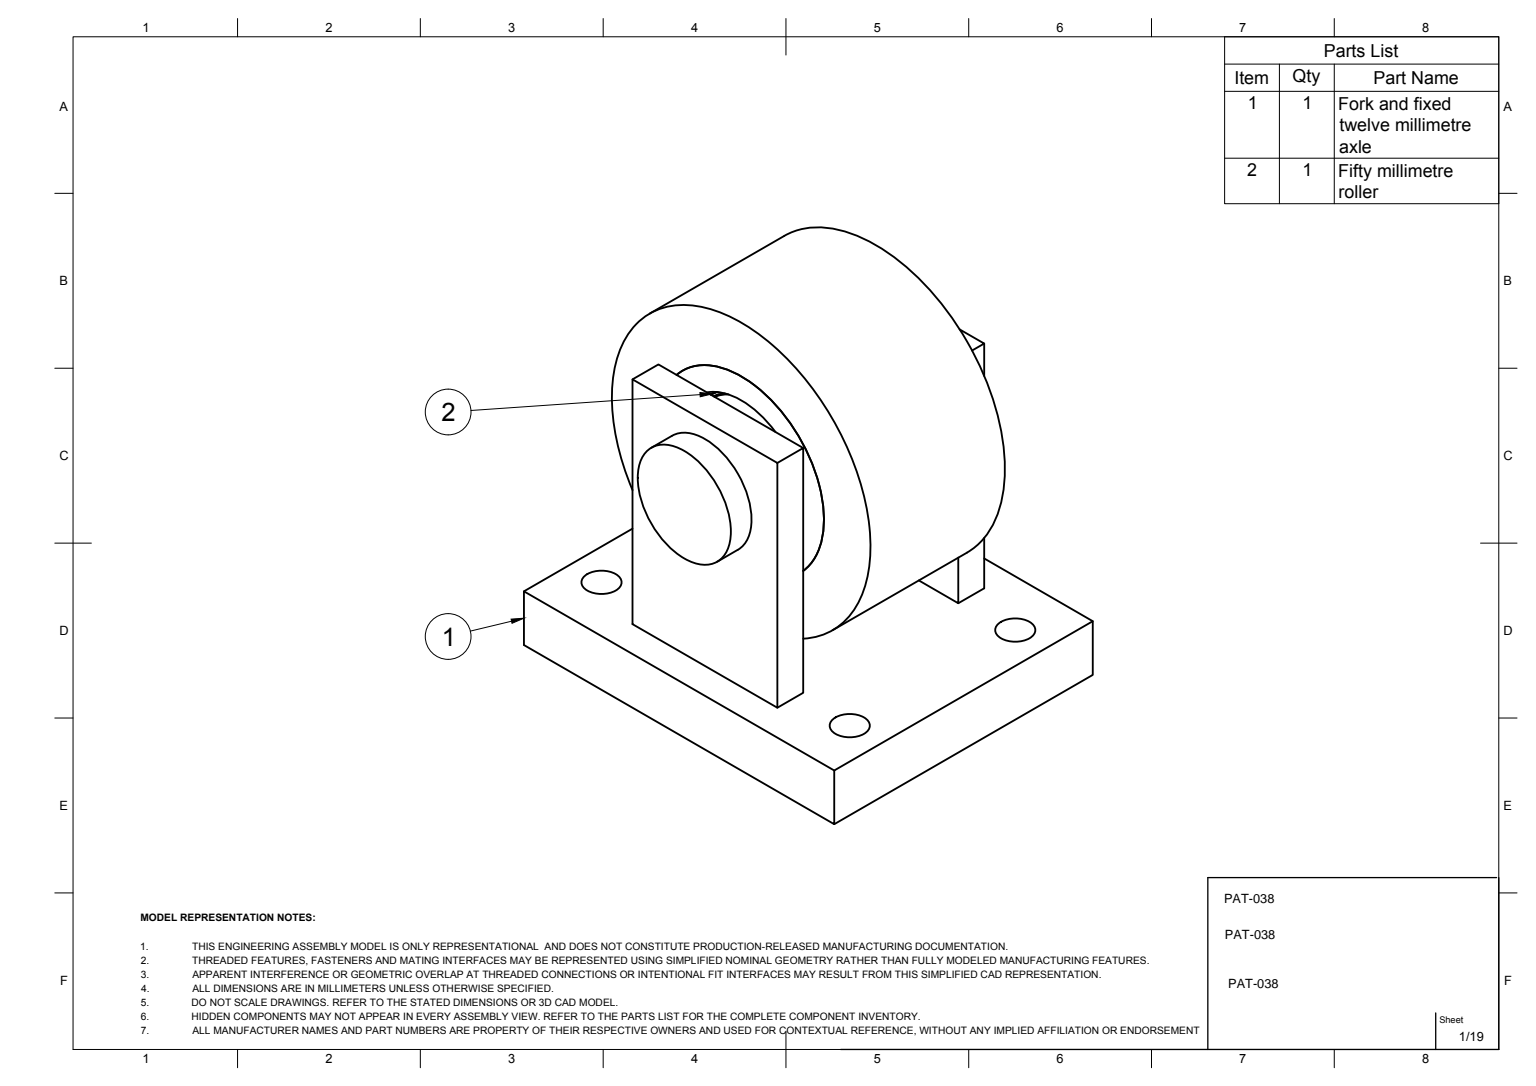
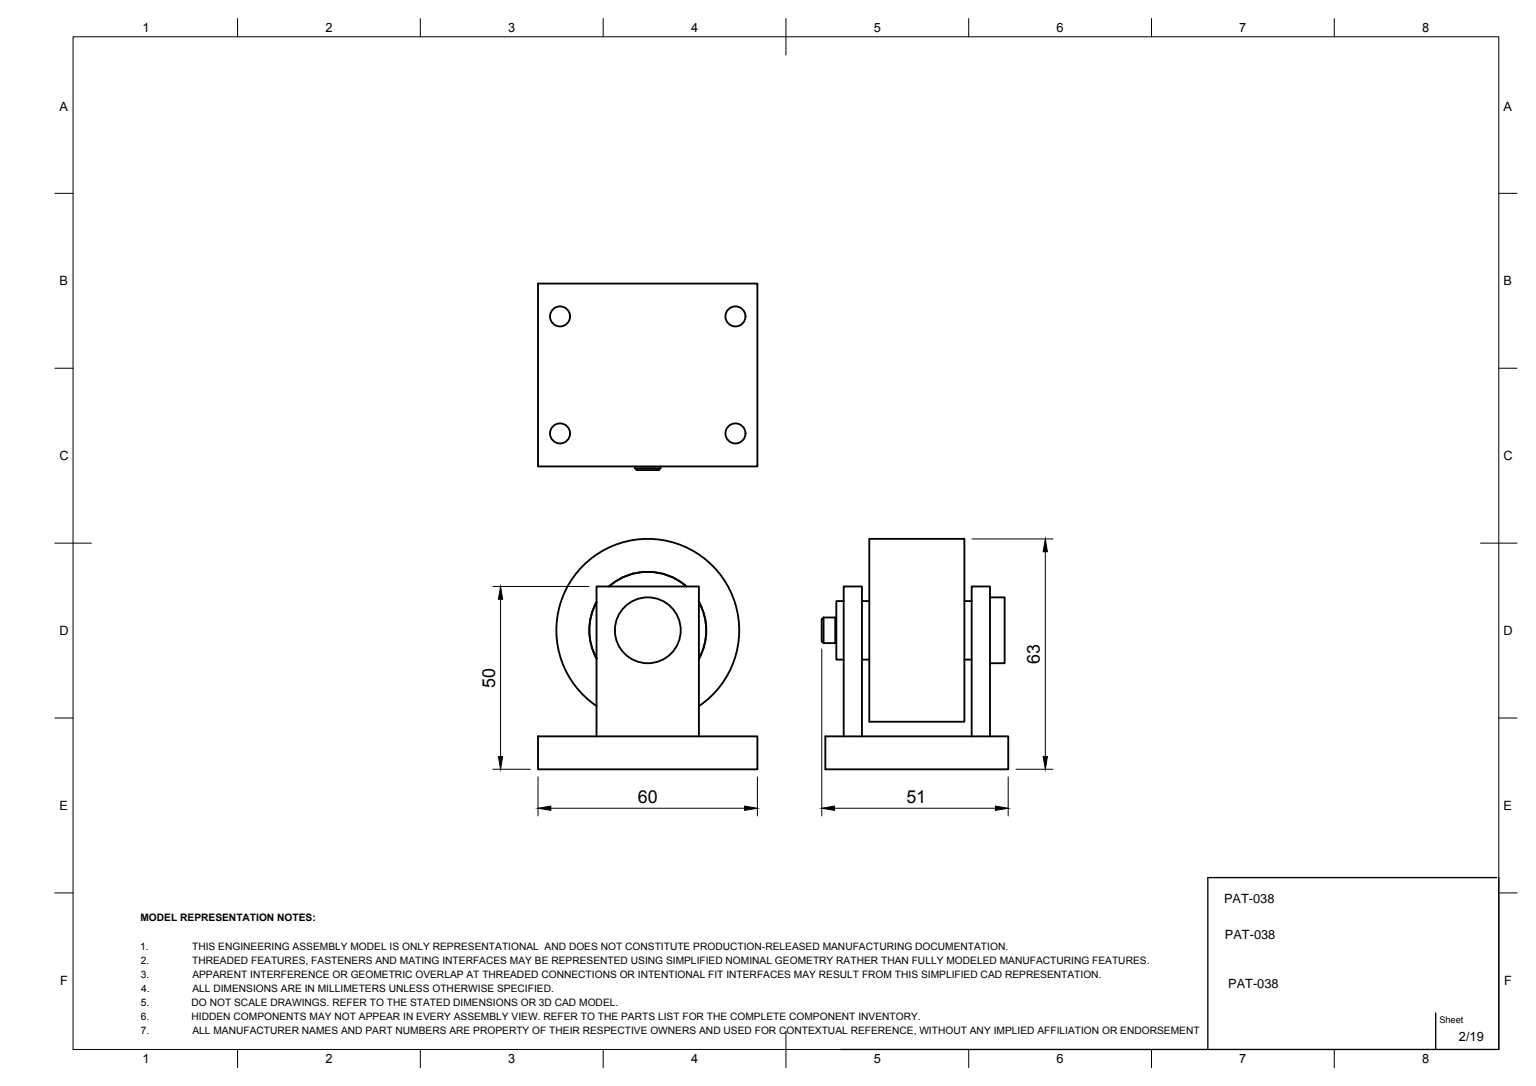
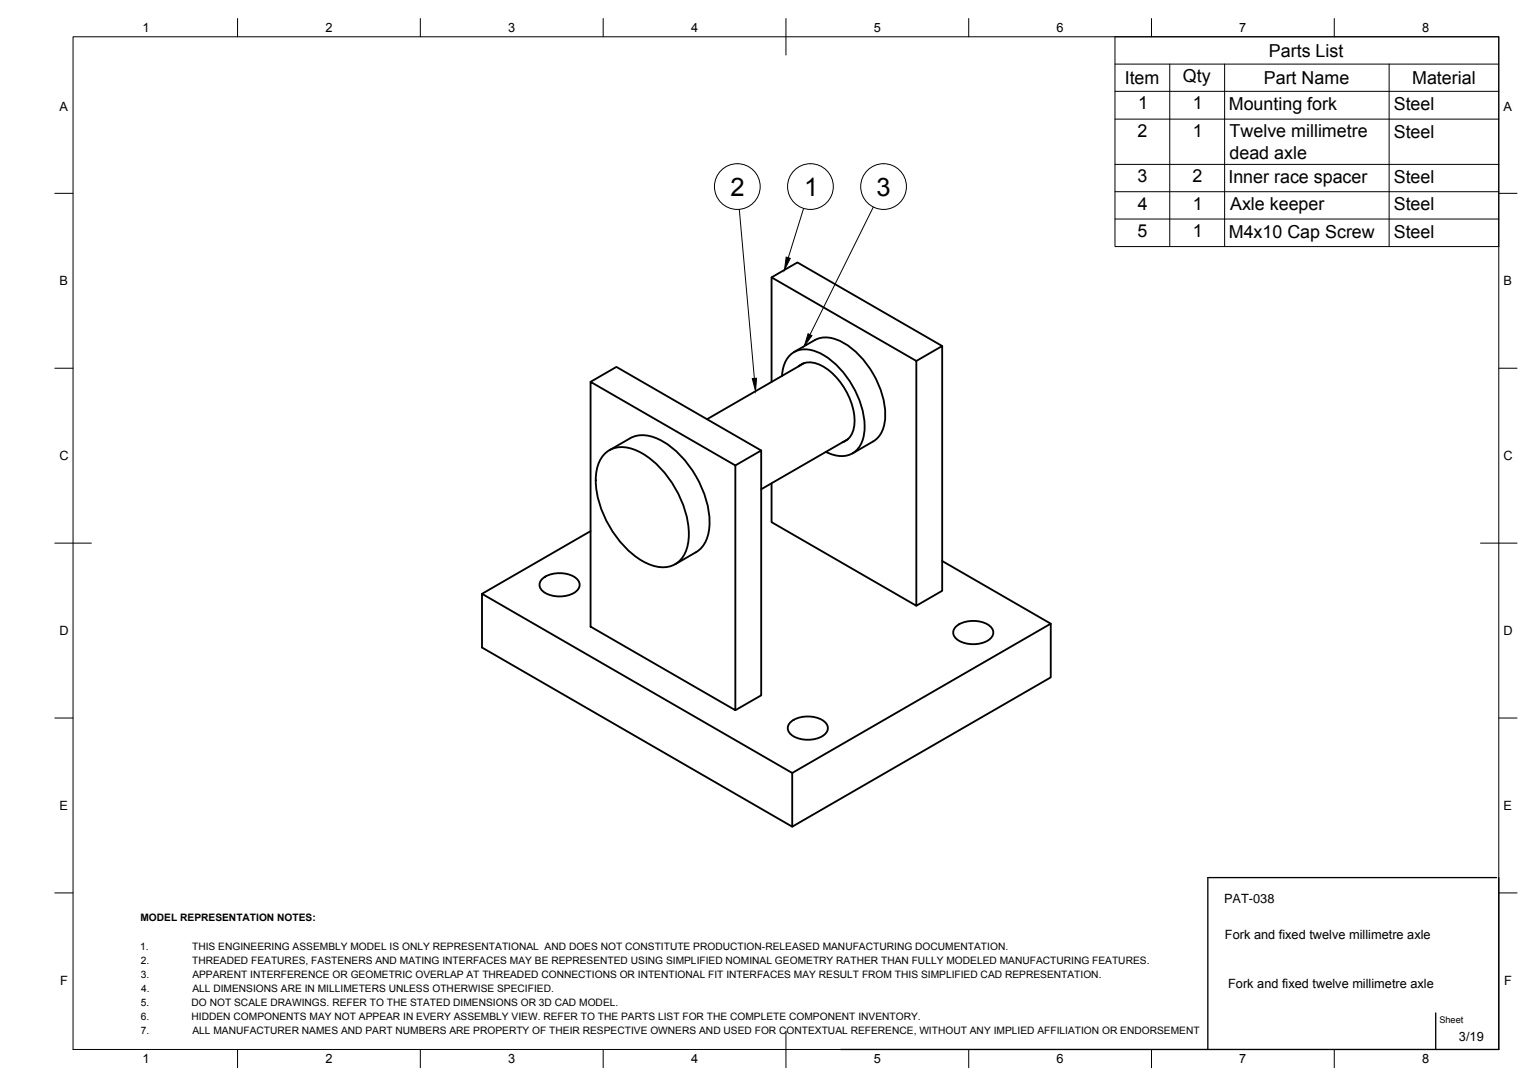
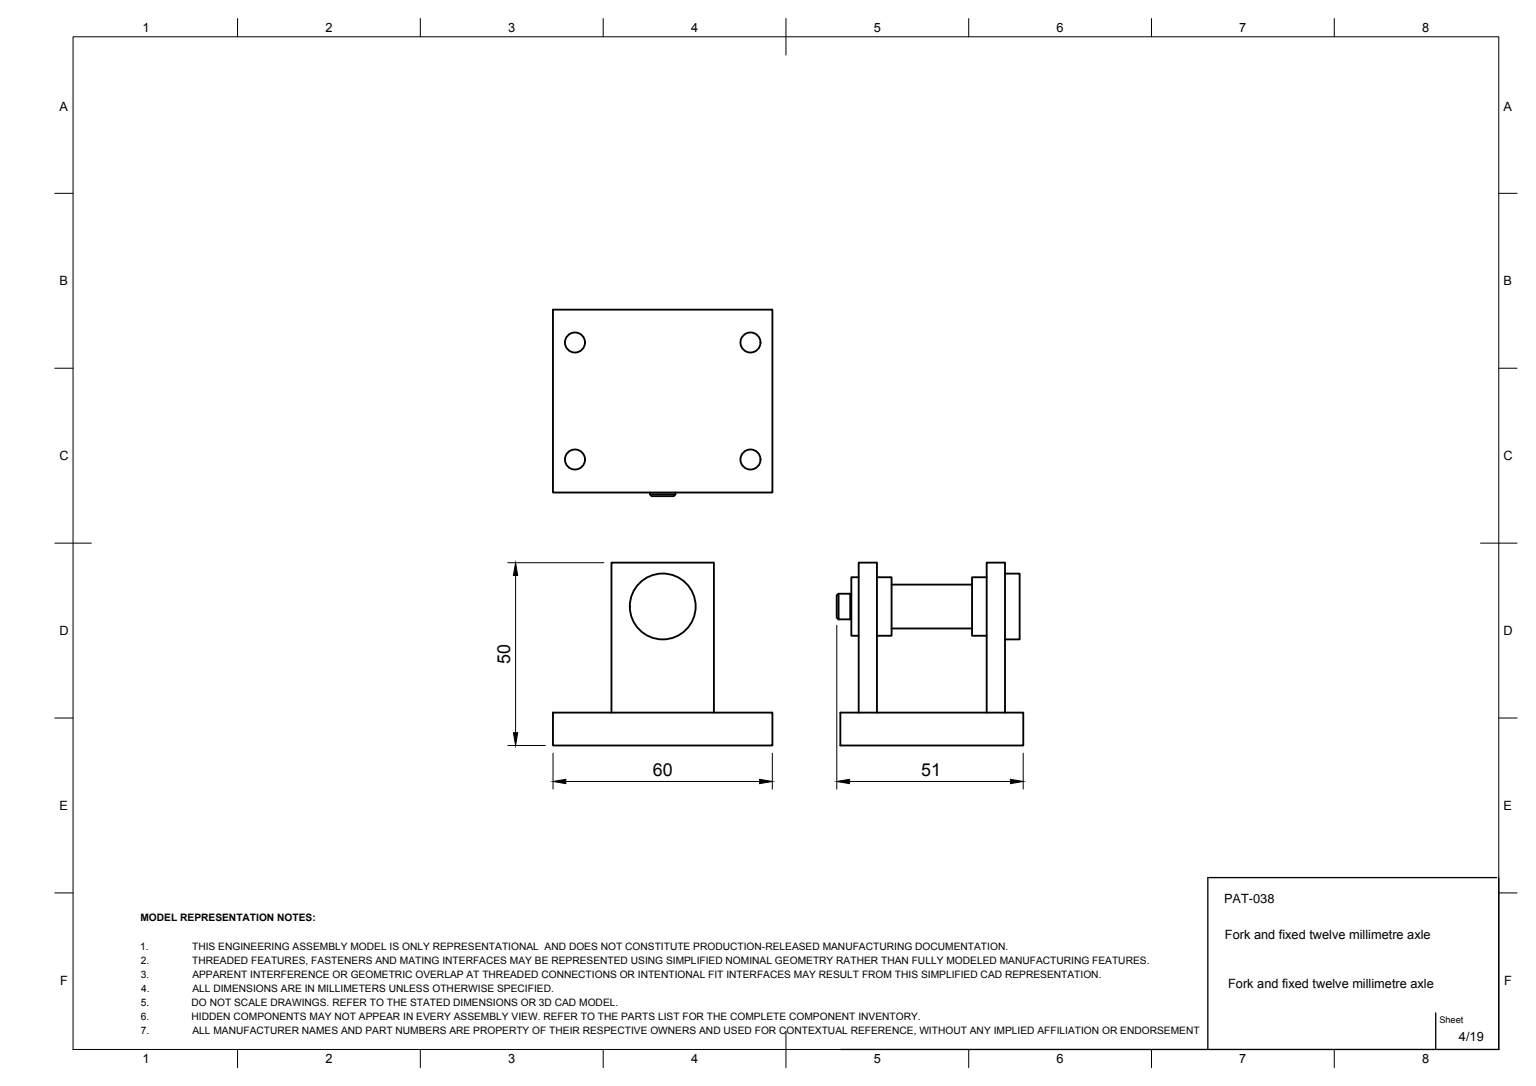
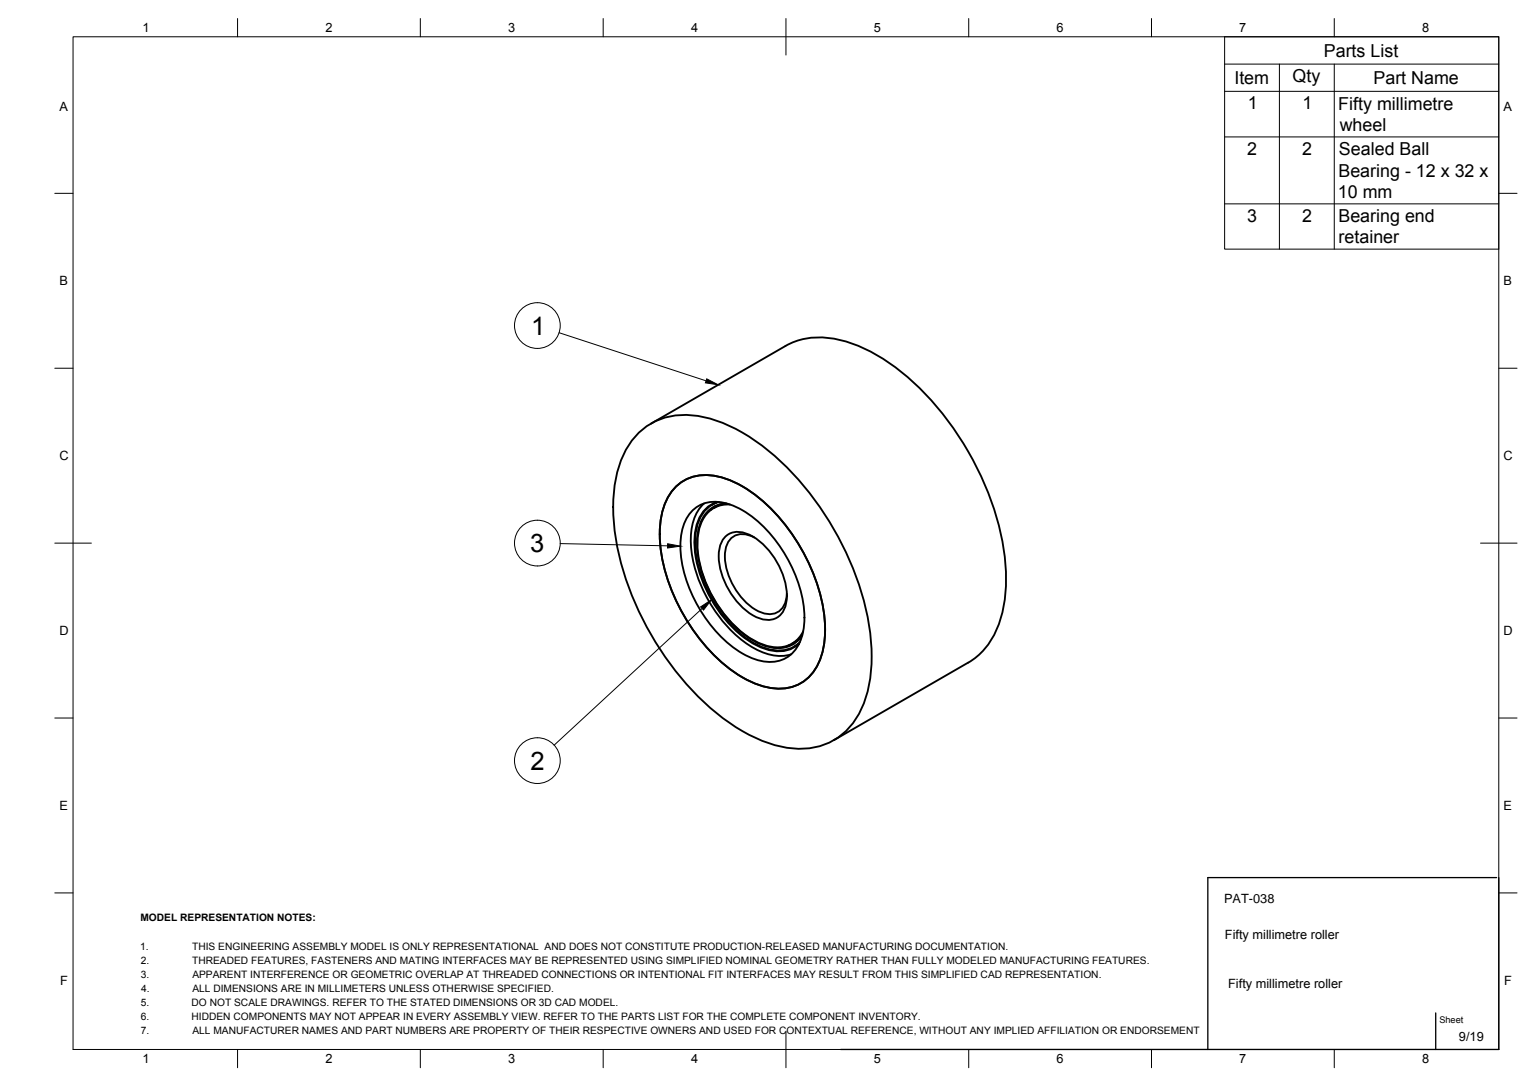
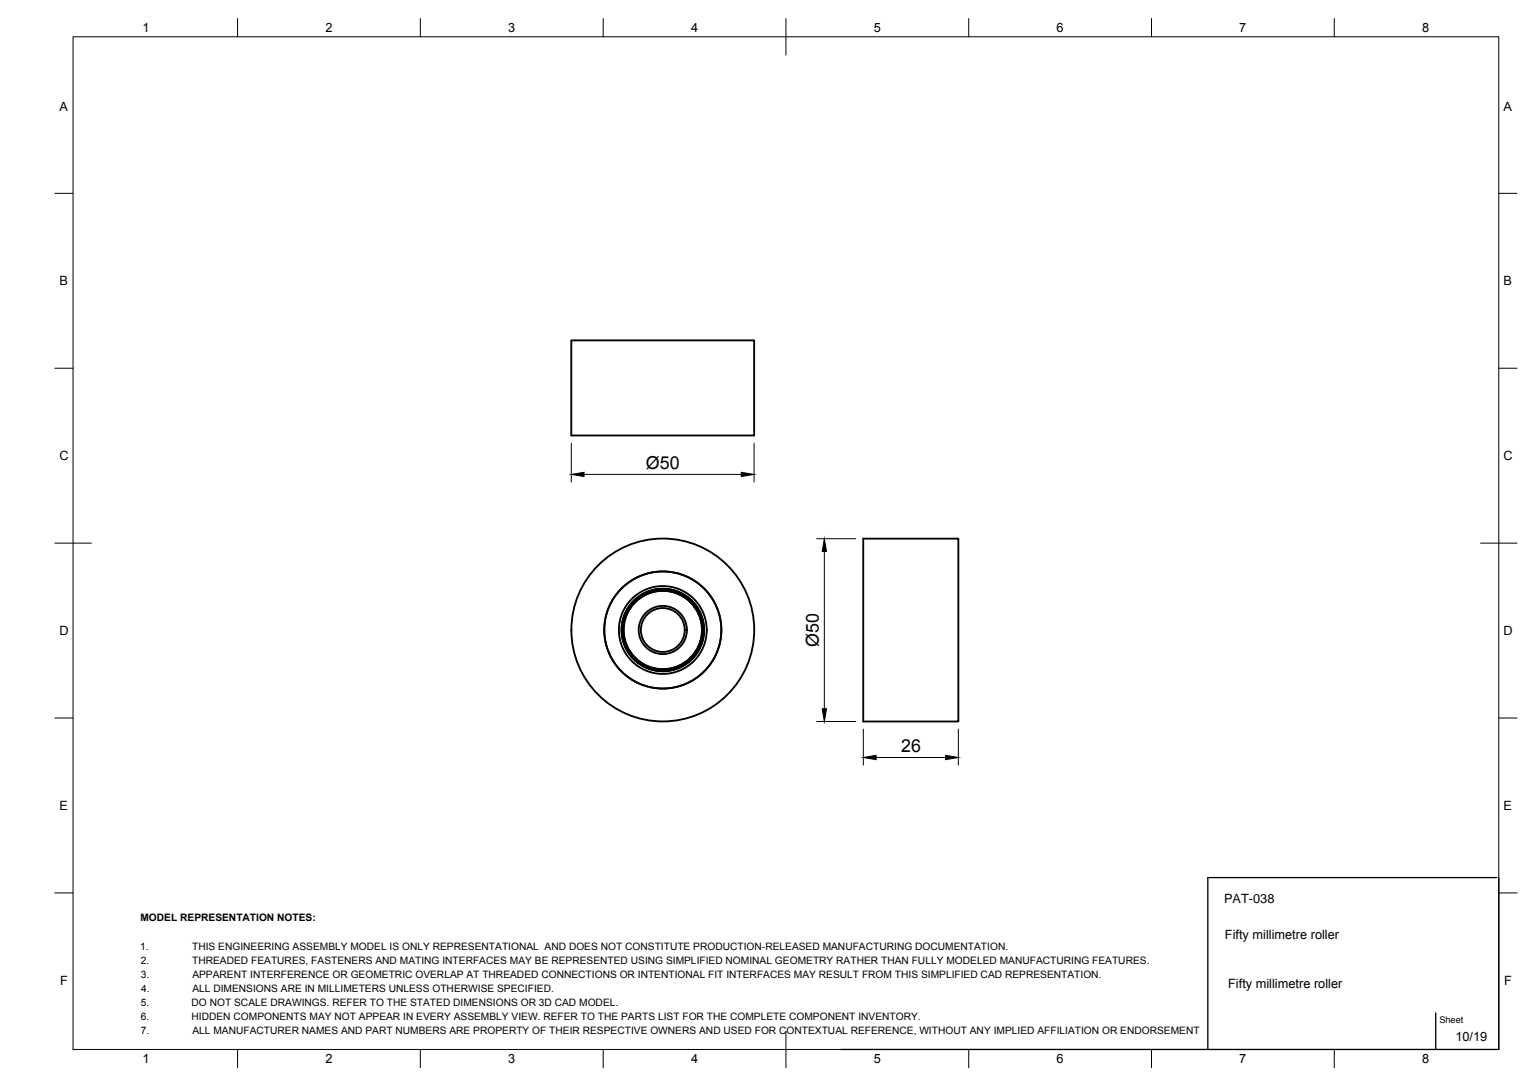
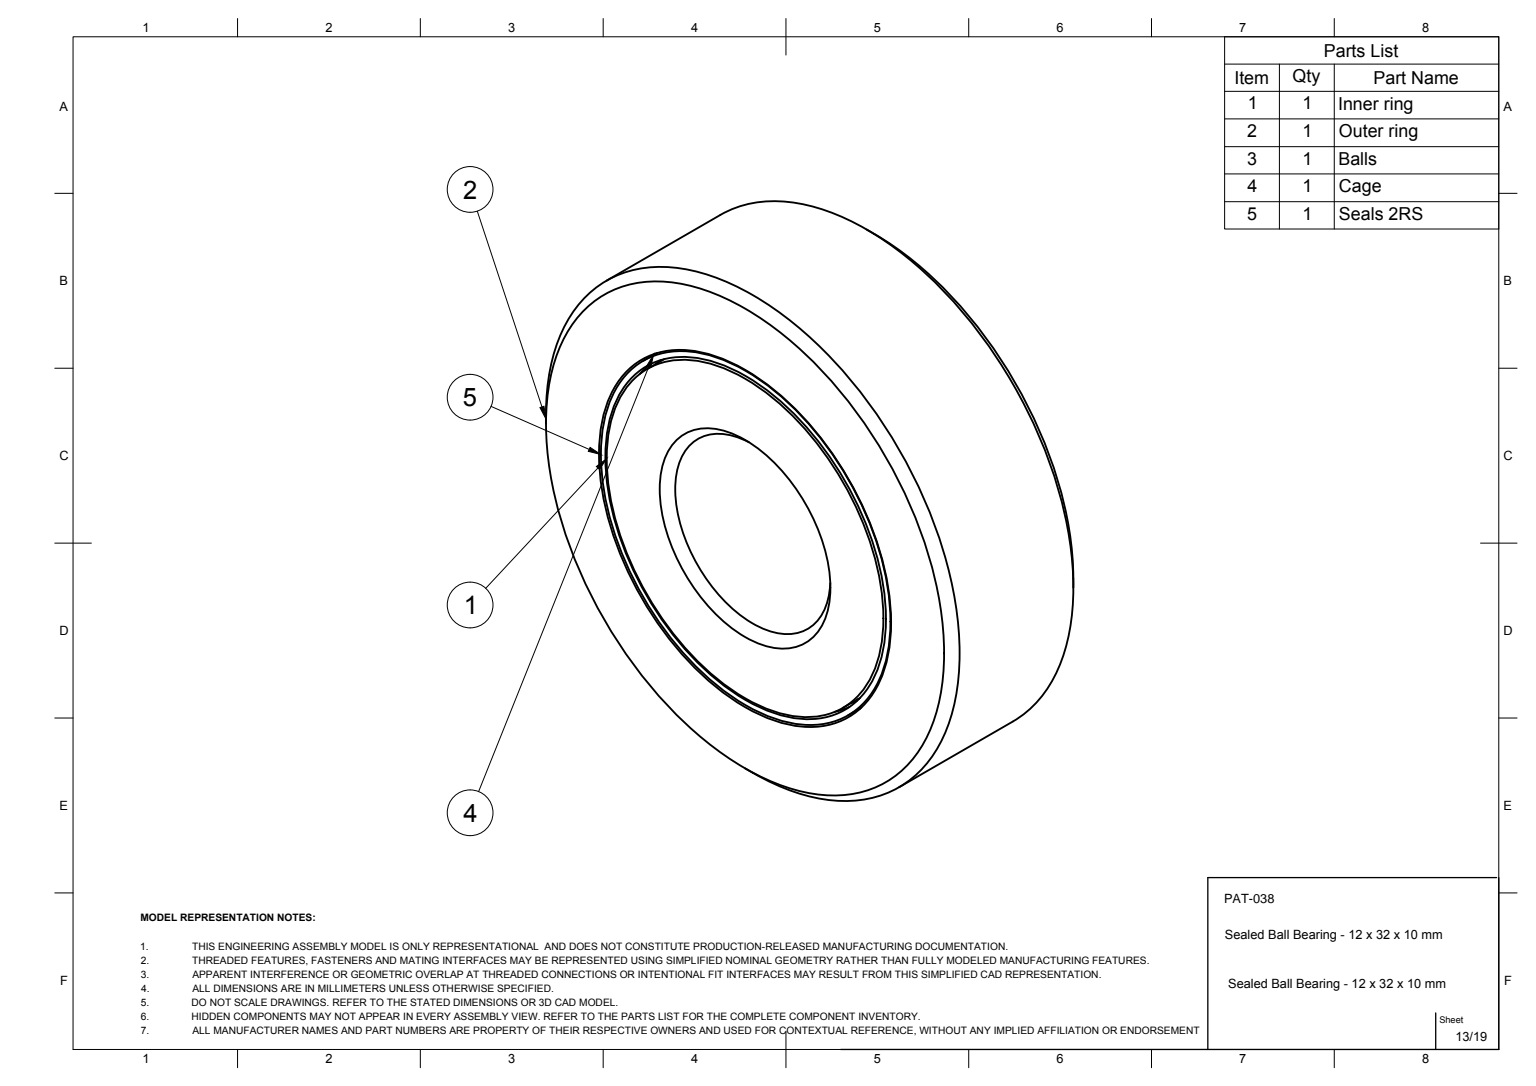
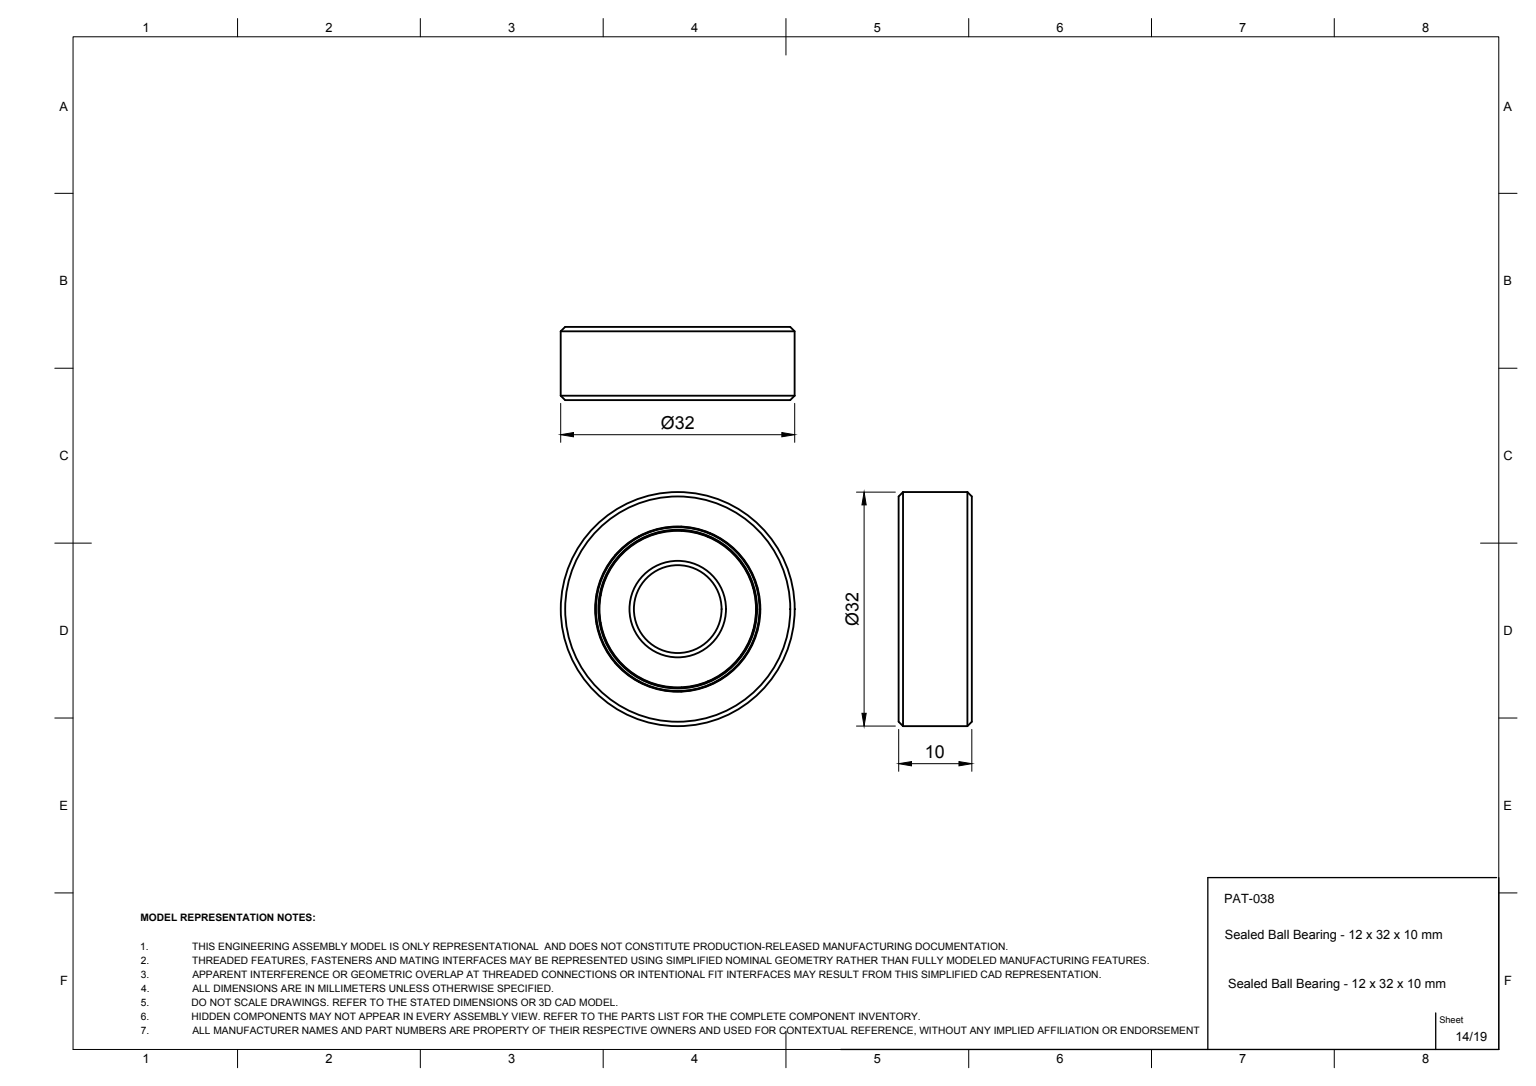
ISO-10303-21;
HEADER;
/* Generated by software containing ST-Developer
 * from STEP Tools, Inc. (www.steptools.com) 
 */

FILE_DESCRIPTION(
/* description */ ('Fork-mounted skate wheel'),
/* implementation_level */ '2;1');

FILE_NAME(
/* name */ 'PAT-038',
/* time_stamp */ '2026-10-29T16:11:26-07:00',
/* author */ (''),
/* organization */ (''),
/* preprocessor_version */ 'ST-DEVELOPER v20.2',
/* originating_system */ 'Autodesk Translation Framework v15.17.0.0',
/* authorisation */ '');

FILE_SCHEMA (('AUTOMOTIVE_DESIGN { 1 0 10303 214 3 1 1 }'));
ENDSEC;

DATA;
#10=MECHANICAL_DESIGN_GEOMETRIC_PRESENTATION_REPRESENTATION('',(#146,#147,
#148,#149,#150,#151,#152,#153,#154,#155,#156,#157,#158,#159,#160,#161,#162,
#163,#164),#3688);
#11=B_SPLINE_CURVE_WITH_KNOTS('',3,(#3211,#3212,#3213,#3214,#3215,#3216,
#3217,#3218,#3219,#3220,#3221,#3222,#3223,#3224,#3225,#3226,#3227,#3228,
#3229,#3230,#3231,#3232),.UNSPECIFIED.,.F.,.F.,(4,2,2,2,2,2,2,2,2,2,4),
(0.0591825211272536,0.157966726598481,0.236950089897721,0.315933453196962,
0.391576304923761,0.46721915665056,0.54286200837736,0.618504860104159,0.697488223403399,
0.77647158670264,0.875255792173867),.UNSPECIFIED.);
#12=B_SPLINE_CURVE_WITH_KNOTS('',3,(#3236,#3237,#3238,#3239,#3240,#3241,
#3242,#3243,#3244,#3245,#3246,#3247,#3248,#3249,#3250,#3251,#3252,#3253,
#3254,#3255,#3256,#3257),.UNSPECIFIED.,.F.,.F.,(4,2,2,2,2,2,2,2,2,2,4),
(0.0581119756758434,0.106553146291161,0.213106292582322,0.30849933801665,
0.386091982889075,0.4636846277615,0.541277272633925,0.61886991750635,0.714262962940678,
0.820816109231839,0.869257279847157),.UNSPECIFIED.);
#13=B_SPLINE_CURVE_WITH_KNOTS('',3,(#3263,#3264,#3265,#3266,#3267,#3268,
#3269,#3270,#3271,#3272,#3273,#3274,#3275,#3276,#3277,#3278,#3279,#3280,
#3281,#3282,#3283,#3284),.UNSPECIFIED.,.F.,.F.,(4,2,2,2,2,2,2,2,2,2,4),
(0.0581119756758434,0.106553146291161,0.213106292582322,0.30849933801665,
0.386091982889075,0.4636846277615,0.541277272633925,0.61886991750635,0.714262962940679,
0.820816109231839,0.869257279847157),.UNSPECIFIED.);
#14=B_SPLINE_CURVE_WITH_KNOTS('',3,(#3288,#3289,#3290,#3291,#3292,#3293,
#3294,#3295,#3296,#3297,#3298,#3299,#3300,#3301,#3302,#3303,#3304,#3305,
#3306,#3307,#3308,#3309),.UNSPECIFIED.,.F.,.F.,(4,2,2,2,2,2,2,2,2,2,4),
(0.0581119756758433,0.106553146291161,0.213106292582322,0.308499338016649,
0.386091982889075,0.4636846277615,0.541277272633925,0.61886991750635,0.714262962940678,
0.820816109231839,0.869257279847157),.UNSPECIFIED.);
#15=B_SPLINE_CURVE_WITH_KNOTS('',3,(#3318,#3319,#3320,#3321,#3322,#3323,
#3324,#3325,#3326,#3327,#3328,#3329,#3330,#3331,#3332,#3333,#3334,#3335,
#3336,#3337,#3338,#3339),.UNSPECIFIED.,.F.,.F.,(4,2,2,2,2,2,2,2,2,2,4),
(0.0581119756758433,0.106553146291161,0.213106292582322,0.30849933801665,
0.386091982889075,0.4636846277615,0.541277272633925,0.61886991750635,0.714262962940678,
0.820816109231839,0.869257279847157),.UNSPECIFIED.);
#16=B_SPLINE_CURVE_WITH_KNOTS('',3,(#3343,#3344,#3345,#3346,#3347,#3348,
#3349,#3350,#3351,#3352,#3353,#3354,#3355,#3356,#3357,#3358,#3359,#3360,
#3361,#3362,#3363,#3364),.UNSPECIFIED.,.F.,.F.,(4,2,2,2,2,2,2,2,2,2,4),
(0.0581119756758434,0.106553146291161,0.213106292582322,0.30849933801665,
0.386091982889075,0.4636846277615,0.541277272633925,0.61886991750635,0.714262962940678,
0.820816109231839,0.869257279847157),.UNSPECIFIED.);
#17=B_SPLINE_CURVE_WITH_KNOTS('',3,(#3368,#3369,#3370,#3371,#3372,#3373,
#3374,#3375,#3376,#3377,#3378,#3379,#3380,#3381,#3382,#3383,#3384,#3385,
#3386,#3387,#3388,#3389),.UNSPECIFIED.,.F.,.F.,(4,2,2,2,2,2,2,2,2,2,4),
(0.0581119756758434,0.106553146291161,0.213106292582322,0.30849933801665,
0.386091982889075,0.4636846277615,0.541277272633925,0.61886991750635,0.714262962940678,
0.820816109231839,0.869257279847157),.UNSPECIFIED.);
#18=B_SPLINE_CURVE_WITH_KNOTS('',3,(#3393,#3394,#3395,#3396,#3397,#3398,
#3399,#3400,#3401,#3402,#3403,#3404,#3405,#3406,#3407,#3408,#3409,#3410,
#3411,#3412,#3413,#3414),.UNSPECIFIED.,.F.,.F.,(4,2,2,2,2,2,2,2,2,2,4),
(0.0581119756758433,0.106553146291161,0.213106292582322,0.30849933801665,
0.386091982889075,0.4636846277615,0.541277272633925,0.61886991750635,0.714262962940678,
0.820816109231839,0.869257279847157),.UNSPECIFIED.);
#19=B_SPLINE_CURVE_WITH_KNOTS('',3,(#3422,#3423,#3424,#3425,#3426,#3427,
#3428,#3429,#3430,#3431,#3432,#3433,#3434,#3435,#3436,#3437,#3438,#3439,
#3440,#3441,#3442,#3443),.UNSPECIFIED.,.F.,.F.,(4,2,2,2,2,2,2,2,2,2,4),
(0.0591825211272536,0.157966726598481,0.236950089897721,0.315933453196962,
0.391576304923761,0.467219156650561,0.54286200837736,0.618504860104159,
0.697488223403399,0.77647158670264,0.875255792173867),.UNSPECIFIED.);
#20=B_SPLINE_CURVE_WITH_KNOTS('',3,(#3451,#3452,#3453,#3454,#3455,#3456,
#3457,#3458,#3459,#3460,#3461,#3462,#3463,#3464,#3465,#3466,#3467,#3468,
#3469,#3470,#3471,#3472),.UNSPECIFIED.,.F.,.F.,(4,2,2,2,2,2,2,2,2,2,4),
(0.0591825211272536,0.157966726598481,0.236950089897722,0.315933453196962,
0.391576304923761,0.467219156650561,0.54286200837736,0.618504860104159,
0.697488223403399,0.77647158670264,0.875255792173867),.UNSPECIFIED.);
#21=B_SPLINE_CURVE_WITH_KNOTS('',3,(#3482,#3483,#3484,#3485,#3486,#3487,
#3488,#3489,#3490,#3491,#3492,#3493,#3494,#3495,#3496,#3497,#3498,#3499,
#3500,#3501,#3502,#3503),.UNSPECIFIED.,.F.,.F.,(4,2,2,2,2,2,2,2,2,2,4),
(0.0591825211272536,0.157966726598481,0.236950089897721,0.315933453196962,
0.391576304923761,0.46721915665056,0.54286200837736,0.618504860104159,0.697488223403399,
0.77647158670264,0.875255792173867),.UNSPECIFIED.);
#22=B_SPLINE_CURVE_WITH_KNOTS('',3,(#3511,#3512,#3513,#3514,#3515,#3516,
#3517,#3518,#3519,#3520,#3521,#3522,#3523,#3524,#3525,#3526,#3527,#3528,
#3529,#3530,#3531,#3532),.UNSPECIFIED.,.F.,.F.,(4,2,2,2,2,2,2,2,2,2,4),
(0.0591825211272536,0.157966726598481,0.236950089897721,0.315933453196962,
0.391576304923761,0.46721915665056,0.542862008377359,0.618504860104159,
0.697488223403399,0.776471586702639,0.875255792173867),.UNSPECIFIED.);
#23=B_SPLINE_CURVE_WITH_KNOTS('',3,(#3540,#3541,#3542,#3543,#3544,#3545,
#3546,#3547,#3548,#3549,#3550,#3551,#3552,#3553,#3554,#3555,#3556,#3557,
#3558,#3559,#3560,#3561),.UNSPECIFIED.,.F.,.F.,(4,2,2,2,2,2,2,2,2,2,4),
(0.0591825211272536,0.157966726598481,0.236950089897721,0.315933453196962,
0.391576304923761,0.46721915665056,0.54286200837736,0.618504860104159,0.697488223403399,
0.77647158670264,0.875255792173867),.UNSPECIFIED.);
#24=B_SPLINE_CURVE_WITH_KNOTS('',3,(#3570,#3571,#3572,#3573,#3574,#3575,
#3576,#3577,#3578,#3579,#3580,#3581,#3582,#3583,#3584,#3585,#3586,#3587,
#3588,#3589,#3590,#3591),.UNSPECIFIED.,.F.,.F.,(4,2,2,2,2,2,2,2,2,2,4),
(0.0591825211272536,0.157966726598481,0.236950089897721,0.315933453196962,
0.391576304923761,0.46721915665056,0.542862008377359,0.618504860104159,
0.697488223403399,0.776471586702639,0.875255792173867),.UNSPECIFIED.);
#25=SPHERICAL_SURFACE('',#2119,0.29765);
#26=SPHERICAL_SURFACE('',#2121,0.29765);
#27=SPHERICAL_SURFACE('',#2123,0.29765);
#28=SPHERICAL_SURFACE('',#2125,0.29765);
#29=SPHERICAL_SURFACE('',#2127,0.29765);
#30=SPHERICAL_SURFACE('',#2129,0.29765);
#31=SPHERICAL_SURFACE('',#2131,0.29765);
#32=SPHERICAL_SURFACE('',#2134,0.309556);
#33=SPHERICAL_SURFACE('',#2150,0.309556);
#34=SPHERICAL_SURFACE('',#2155,0.309556);
#35=SPHERICAL_SURFACE('',#2161,0.309556);
#36=SPHERICAL_SURFACE('',#2166,0.309556);
#37=SPHERICAL_SURFACE('',#2171,0.309556);
#38=SPHERICAL_SURFACE('',#2179,0.309556);
#39=TOROIDAL_SURFACE('',#2079,1.1,0.309556);
#40=TOROIDAL_SURFACE('',#2099,1.1,0.309556);
#41=ITEM_DEFINED_TRANSFORMATION($,$,#1962,#2053);
#42=ITEM_DEFINED_TRANSFORMATION($,$,#1997,#2054);
#43=ITEM_DEFINED_TRANSFORMATION($,$,#2011,#2055);
#44=ITEM_DEFINED_TRANSFORMATION($,$,#2011,#2056);
#45=ITEM_DEFINED_TRANSFORMATION($,$,#2020,#2057);
#46=ITEM_DEFINED_TRANSFORMATION($,$,#2029,#2058);
#47=ITEM_DEFINED_TRANSFORMATION($,$,#2078,#2200);
#48=ITEM_DEFINED_TRANSFORMATION($,$,#2098,#2201);
#49=ITEM_DEFINED_TRANSFORMATION($,$,#2118,#2202);
#50=ITEM_DEFINED_TRANSFORMATION($,$,#2133,#2203);
#51=ITEM_DEFINED_TRANSFORMATION($,$,#2183,#2204);
#52=ITEM_DEFINED_TRANSFORMATION($,$,#2060,#2214);
#53=ITEM_DEFINED_TRANSFORMATION($,$,#2205,#2215);
#54=ITEM_DEFINED_TRANSFORMATION($,$,#2077,#2216);
#55=ITEM_DEFINED_TRANSFORMATION($,$,#2077,#2217);
#56=ITEM_DEFINED_TRANSFORMATION($,$,#2205,#2218);
#57=ITEM_DEFINED_TRANSFORMATION($,$,#1961,#2219);
#58=ITEM_DEFINED_TRANSFORMATION($,$,#2059,#2220);
#59=(
REPRESENTATION_RELATIONSHIP($,$,#3745,#3744)
REPRESENTATION_RELATIONSHIP_WITH_TRANSFORMATION(#41)
SHAPE_REPRESENTATION_RELATIONSHIP()
);
#60=(
REPRESENTATION_RELATIONSHIP($,$,#3746,#3744)
REPRESENTATION_RELATIONSHIP_WITH_TRANSFORMATION(#42)
SHAPE_REPRESENTATION_RELATIONSHIP()
);
#61=(
REPRESENTATION_RELATIONSHIP($,$,#3747,#3744)
REPRESENTATION_RELATIONSHIP_WITH_TRANSFORMATION(#43)
SHAPE_REPRESENTATION_RELATIONSHIP()
);
#62=(
REPRESENTATION_RELATIONSHIP($,$,#3747,#3744)
REPRESENTATION_RELATIONSHIP_WITH_TRANSFORMATION(#44)
SHAPE_REPRESENTATION_RELATIONSHIP()
);
#63=(
REPRESENTATION_RELATIONSHIP($,$,#3748,#3744)
REPRESENTATION_RELATIONSHIP_WITH_TRANSFORMATION(#45)
SHAPE_REPRESENTATION_RELATIONSHIP()
);
#64=(
REPRESENTATION_RELATIONSHIP($,$,#3749,#3744)
REPRESENTATION_RELATIONSHIP_WITH_TRANSFORMATION(#46)
SHAPE_REPRESENTATION_RELATIONSHIP()
);
#65=(
REPRESENTATION_RELATIONSHIP($,$,#3753,#3752)
REPRESENTATION_RELATIONSHIP_WITH_TRANSFORMATION(#47)
SHAPE_REPRESENTATION_RELATIONSHIP()
);
#66=(
REPRESENTATION_RELATIONSHIP($,$,#3754,#3752)
REPRESENTATION_RELATIONSHIP_WITH_TRANSFORMATION(#48)
SHAPE_REPRESENTATION_RELATIONSHIP()
);
#67=(
REPRESENTATION_RELATIONSHIP($,$,#3755,#3752)
REPRESENTATION_RELATIONSHIP_WITH_TRANSFORMATION(#49)
SHAPE_REPRESENTATION_RELATIONSHIP()
);
#68=(
REPRESENTATION_RELATIONSHIP($,$,#3756,#3752)
REPRESENTATION_RELATIONSHIP_WITH_TRANSFORMATION(#50)
SHAPE_REPRESENTATION_RELATIONSHIP()
);
#69=(
REPRESENTATION_RELATIONSHIP($,$,#3757,#3752)
REPRESENTATION_RELATIONSHIP_WITH_TRANSFORMATION(#51)
SHAPE_REPRESENTATION_RELATIONSHIP()
);
#70=(
REPRESENTATION_RELATIONSHIP($,$,#3751,#3750)
REPRESENTATION_RELATIONSHIP_WITH_TRANSFORMATION(#52)
SHAPE_REPRESENTATION_RELATIONSHIP()
);
#71=(
REPRESENTATION_RELATIONSHIP($,$,#3758,#3750)
REPRESENTATION_RELATIONSHIP_WITH_TRANSFORMATION(#53)
SHAPE_REPRESENTATION_RELATIONSHIP()
);
#72=(
REPRESENTATION_RELATIONSHIP($,$,#3752,#3750)
REPRESENTATION_RELATIONSHIP_WITH_TRANSFORMATION(#54)
SHAPE_REPRESENTATION_RELATIONSHIP()
);
#73=(
REPRESENTATION_RELATIONSHIP($,$,#3752,#3750)
REPRESENTATION_RELATIONSHIP_WITH_TRANSFORMATION(#55)
SHAPE_REPRESENTATION_RELATIONSHIP()
);
#74=(
REPRESENTATION_RELATIONSHIP($,$,#3758,#3750)
REPRESENTATION_RELATIONSHIP_WITH_TRANSFORMATION(#56)
SHAPE_REPRESENTATION_RELATIONSHIP()
);
#75=(
REPRESENTATION_RELATIONSHIP($,$,#3744,#3743)
REPRESENTATION_RELATIONSHIP_WITH_TRANSFORMATION(#57)
SHAPE_REPRESENTATION_RELATIONSHIP()
);
#76=(
REPRESENTATION_RELATIONSHIP($,$,#3750,#3743)
REPRESENTATION_RELATIONSHIP_WITH_TRANSFORMATION(#58)
SHAPE_REPRESENTATION_RELATIONSHIP()
);
#77=CONTEXT_DEPENDENT_SHAPE_REPRESENTATION(#59,#3716);
#78=CONTEXT_DEPENDENT_SHAPE_REPRESENTATION(#60,#3717);
#79=CONTEXT_DEPENDENT_SHAPE_REPRESENTATION(#61,#3718);
#80=CONTEXT_DEPENDENT_SHAPE_REPRESENTATION(#62,#3719);
#81=CONTEXT_DEPENDENT_SHAPE_REPRESENTATION(#63,#3720);
#82=CONTEXT_DEPENDENT_SHAPE_REPRESENTATION(#64,#3721);
#83=CONTEXT_DEPENDENT_SHAPE_REPRESENTATION(#65,#3730);
#84=CONTEXT_DEPENDENT_SHAPE_REPRESENTATION(#66,#3731);
#85=CONTEXT_DEPENDENT_SHAPE_REPRESENTATION(#67,#3732);
#86=CONTEXT_DEPENDENT_SHAPE_REPRESENTATION(#68,#3733);
#87=CONTEXT_DEPENDENT_SHAPE_REPRESENTATION(#69,#3734);
#88=CONTEXT_DEPENDENT_SHAPE_REPRESENTATION(#70,#3736);
#89=CONTEXT_DEPENDENT_SHAPE_REPRESENTATION(#71,#3737);
#90=CONTEXT_DEPENDENT_SHAPE_REPRESENTATION(#72,#3738);
#91=CONTEXT_DEPENDENT_SHAPE_REPRESENTATION(#73,#3739);
#92=CONTEXT_DEPENDENT_SHAPE_REPRESENTATION(#74,#3740);
#93=CONTEXT_DEPENDENT_SHAPE_REPRESENTATION(#75,#3741);
#94=CONTEXT_DEPENDENT_SHAPE_REPRESENTATION(#76,#3742);
#95=NEXT_ASSEMBLY_USAGE_OCCURRENCE('Mounting fork:1','Mounting fork:1',
'Mounting fork:1',#3761,#3762,'Mounting fork:1');
#96=NEXT_ASSEMBLY_USAGE_OCCURRENCE('Twelve millimetre dead axle:1',
'Twelve millimetre dead axle:1','Twelve millimetre dead axle:1',#3761,#3763,
'Twelve millimetre dead axle:1');
#97=NEXT_ASSEMBLY_USAGE_OCCURRENCE('Inner race spacer:2',
'Inner race spacer:2','Inner race spacer:2',#3761,#3764,
'Inner race spacer:2');
#98=NEXT_ASSEMBLY_USAGE_OCCURRENCE('Inner race spacer:3',
'Inner race spacer:3','Inner race spacer:3',#3761,#3764,
'Inner race spacer:3');
#99=NEXT_ASSEMBLY_USAGE_OCCURRENCE('Axle keeper:2','Axle keeper:2',
'Axle keeper:2',#3761,#3765,'Axle keeper:2');
#100=NEXT_ASSEMBLY_USAGE_OCCURRENCE('M4x10 Cap Screw:2',
'M4x10 Cap Screw:2','M4x10 Cap Screw:2',#3761,#3766,'M4x10 Cap Screw:2');
#101=NEXT_ASSEMBLY_USAGE_OCCURRENCE('Inner ring:1','Inner ring:1',
'Inner ring:1',#3769,#3770,'Inner ring:1');
#102=NEXT_ASSEMBLY_USAGE_OCCURRENCE('Outer ring:1','Outer ring:1',
'Outer ring:1',#3769,#3771,'Outer ring:1');
#103=NEXT_ASSEMBLY_USAGE_OCCURRENCE('Balls:1','Balls:1','Balls:1',#3769,
#3772,'Balls:1');
#104=NEXT_ASSEMBLY_USAGE_OCCURRENCE('Cage:1','Cage:1','Cage:1',#3769,#3773,
'Cage:1');
#105=NEXT_ASSEMBLY_USAGE_OCCURRENCE('Seals 2RS:1','Seals 2RS:1',
'Seals 2RS:1',#3769,#3774,'Seals 2RS:1');
#106=NEXT_ASSEMBLY_USAGE_OCCURRENCE('Fifty millimetre wheel:1',
'Fifty millimetre wheel:1','Fifty millimetre wheel:1',#3767,#3768,
'Fifty millimetre wheel:1');
#107=NEXT_ASSEMBLY_USAGE_OCCURRENCE('Bearing end retainer:1',
'Bearing end retainer:1','Bearing end retainer:1',#3767,#3775,
'Bearing end retainer:1');
#108=NEXT_ASSEMBLY_USAGE_OCCURRENCE(
'Sealed Ball Bearing - 12 x 32 x 10 mm:2',
'Sealed Ball Bearing - 12 x 32 x 10 mm:2',
'Sealed Ball Bearing - 12 x 32 x 10 mm:2',#3767,#3769,
'Sealed Ball Bearing - 12 x 32 x 10 mm:2');
#109=NEXT_ASSEMBLY_USAGE_OCCURRENCE(
'Sealed Ball Bearing - 12 x 32 x 10 mm:3',
'Sealed Ball Bearing - 12 x 32 x 10 mm:3',
'Sealed Ball Bearing - 12 x 32 x 10 mm:3',#3767,#3769,
'Sealed Ball Bearing - 12 x 32 x 10 mm:3');
#110=NEXT_ASSEMBLY_USAGE_OCCURRENCE('Bearing end retainer:2',
'Bearing end retainer:2','Bearing end retainer:2',#3767,#3775,
'Bearing end retainer:2');
#111=NEXT_ASSEMBLY_USAGE_OCCURRENCE(
'Fork and fixed twelve millimetre axle:1',
'Fork and fixed twelve millimetre axle:1',
'Fork and fixed twelve millimetre axle:1',#3760,#3761,
'Fork and fixed twelve millimetre axle:1');
#112=NEXT_ASSEMBLY_USAGE_OCCURRENCE('Fifty millimetre roller:1',
'Fifty millimetre roller:1','Fifty millimetre roller:1',#3760,#3767,
'Fifty millimetre roller:1');
#113=CONICAL_SURFACE('',#2042,0.325,0.785398163397448);
#114=CONICAL_SURFACE('',#2046,0.335,0.785398163397448);
#115=CONICAL_SURFACE('',#2050,0.21,0.463647609000806);
#116=CONICAL_SURFACE('',#2090,0.63,0.785398163397448);
#117=CONICAL_SURFACE('',#2097,0.63,0.785398163397448);
#118=CONICAL_SURFACE('',#2110,1.57,0.785398163397449);
#119=CONICAL_SURFACE('',#2114,1.57,0.785398163397449);
#120=ORIENTED_CLOSED_SHELL('',*,#1811,.F.);
#121=BREP_WITH_VOIDS('Body1',#1812,(#120));
#122=SHAPE_REPRESENTATION_RELATIONSHIP('SRR','None',#3745,#134);
#123=SHAPE_REPRESENTATION_RELATIONSHIP('SRR','None',#3746,#135);
#124=SHAPE_REPRESENTATION_RELATIONSHIP('SRR','None',#3747,#136);
#125=SHAPE_REPRESENTATION_RELATIONSHIP('SRR','None',#3748,#137);
#126=SHAPE_REPRESENTATION_RELATIONSHIP('SRR','None',#3749,#138);
#127=SHAPE_REPRESENTATION_RELATIONSHIP('SRR','None',#3751,#139);
#128=SHAPE_REPRESENTATION_RELATIONSHIP('SRR','None',#3753,#140);
#129=SHAPE_REPRESENTATION_RELATIONSHIP('SRR','None',#3754,#141);
#130=SHAPE_REPRESENTATION_RELATIONSHIP('SRR','None',#3755,#142);
#131=SHAPE_REPRESENTATION_RELATIONSHIP('SRR','None',#3756,#143);
#132=SHAPE_REPRESENTATION_RELATIONSHIP('SRR','None',#3757,#144);
#133=SHAPE_REPRESENTATION_RELATIONSHIP('SRR','None',#3758,#145);
#134=ADVANCED_BREP_SHAPE_REPRESENTATION('',(#165),#3674);
#135=ADVANCED_BREP_SHAPE_REPRESENTATION('',(#166),#3675);
#136=ADVANCED_BREP_SHAPE_REPRESENTATION('',(#167),#3676);
#137=ADVANCED_BREP_SHAPE_REPRESENTATION('',(#168),#3677);
#138=ADVANCED_BREP_SHAPE_REPRESENTATION('',(#121),#3678);
#139=ADVANCED_BREP_SHAPE_REPRESENTATION('',(#169),#3680);
#140=ADVANCED_BREP_SHAPE_REPRESENTATION('',(#170),#3682);
#141=ADVANCED_BREP_SHAPE_REPRESENTATION('',(#171),#3683);
#142=ADVANCED_BREP_SHAPE_REPRESENTATION('',(#172,#173,#174,#175,#176,#177,
#178),#3684);
#143=ADVANCED_BREP_SHAPE_REPRESENTATION('',(#179),#3685);
#144=ADVANCED_BREP_SHAPE_REPRESENTATION('',(#180,#181),#3686);
#145=ADVANCED_BREP_SHAPE_REPRESENTATION('',(#182),#3687);
#146=STYLED_ITEM('',(#3882),#165);
#147=STYLED_ITEM('',(#3896),#166);
#148=STYLED_ITEM('',(#3896),#167);
#149=STYLED_ITEM('',(#3896),#168);
#150=STYLED_ITEM('',(#3903),#121);
#151=STYLED_ITEM('',(#3882),#169);
#152=STYLED_ITEM('',(#3896),#170);
#153=STYLED_ITEM('',(#3896),#171);
#154=STYLED_ITEM('',(#3896),#172);
#155=STYLED_ITEM('',(#3896),#173);
#156=STYLED_ITEM('',(#3896),#174);
#157=STYLED_ITEM('',(#3896),#175);
#158=STYLED_ITEM('',(#3896),#176);
#159=STYLED_ITEM('',(#3896),#177);
#160=STYLED_ITEM('',(#3896),#178);
#161=STYLED_ITEM('',(#3896),#179);
#162=STYLED_ITEM('',(#3896),#180);
#163=STYLED_ITEM('',(#3896),#181);
#164=STYLED_ITEM('',(#3896),#182);
#165=MANIFOLD_SOLID_BREP('Body1',#1807);
#166=MANIFOLD_SOLID_BREP('Body1',#1808);
#167=MANIFOLD_SOLID_BREP('Body1',#1809);
#168=MANIFOLD_SOLID_BREP('Body1',#1810);
#169=MANIFOLD_SOLID_BREP('Body1',#1813);
#170=MANIFOLD_SOLID_BREP('Body1',#1814);
#171=MANIFOLD_SOLID_BREP('Body1',#1815);
#172=MANIFOLD_SOLID_BREP('Body1',#1816);
#173=MANIFOLD_SOLID_BREP('Body2',#1817);
#174=MANIFOLD_SOLID_BREP('Body3',#1818);
#175=MANIFOLD_SOLID_BREP('Body4',#1819);
#176=MANIFOLD_SOLID_BREP('Body5',#1820);
#177=MANIFOLD_SOLID_BREP('Body6',#1821);
#178=MANIFOLD_SOLID_BREP('Body7',#1822);
#179=MANIFOLD_SOLID_BREP('Continuous crown cage',#1823);
#180=MANIFOLD_SOLID_BREP('Body1',#1824);
#181=MANIFOLD_SOLID_BREP('Body2',#1825);
#182=MANIFOLD_SOLID_BREP('Body1',#1826);
#183=FACE_BOUND('',#396,.T.);
#184=FACE_BOUND('',#401,.T.);
#185=FACE_BOUND('',#403,.T.);
#186=FACE_BOUND('',#408,.T.);
#187=FACE_BOUND('',#414,.T.);
#188=FACE_BOUND('',#415,.T.);
#189=FACE_BOUND('',#416,.T.);
#190=FACE_BOUND('',#417,.T.);
#191=FACE_BOUND('',#418,.T.);
#192=FACE_BOUND('',#419,.T.);
#193=FACE_BOUND('',#421,.T.);
#194=FACE_BOUND('',#422,.T.);
#195=FACE_BOUND('',#423,.T.);
#196=FACE_BOUND('',#424,.T.);
#197=FACE_BOUND('',#428,.T.);
#198=FACE_BOUND('',#433,.T.);
#199=FACE_BOUND('',#437,.T.);
#200=FACE_BOUND('',#439,.T.);
#201=FACE_BOUND('',#443,.T.);
#202=FACE_BOUND('',#445,.T.);
#203=FACE_BOUND('',#460,.T.);
#204=FACE_BOUND('',#465,.T.);
#205=FACE_BOUND('',#468,.T.);
#206=FACE_BOUND('',#472,.T.);
#207=FACE_BOUND('',#474,.T.);
#208=FACE_BOUND('',#480,.T.);
#209=FACE_BOUND('',#483,.T.);
#210=FACE_BOUND('',#488,.T.);
#211=FACE_BOUND('',#493,.T.);
#212=FACE_BOUND('',#518,.T.);
#213=FACE_BOUND('',#521,.T.);
#214=FACE_BOUND('',#524,.T.);
#215=FACE_BOUND('',#527,.T.);
#216=FACE_BOUND('',#530,.T.);
#217=FACE_BOUND('',#535,.T.);
#218=FACE_BOUND('',#537,.T.);
#219=PLANE('',#1981);
#220=PLANE('',#1982);
#221=PLANE('',#1983);
#222=PLANE('',#1984);
#223=PLANE('',#1985);
#224=PLANE('',#1986);
#225=PLANE('',#1987);
#226=PLANE('',#1988);
#227=PLANE('',#1989);
#228=PLANE('',#1990);
#229=PLANE('',#1991);
#230=PLANE('',#1992);
#231=PLANE('',#1993);
#232=PLANE('',#1994);
#233=PLANE('',#1995);
#234=PLANE('',#1996);
#235=PLANE('',#2001);
#236=PLANE('',#2002);
#237=PLANE('',#2007);
#238=PLANE('',#2010);
#239=PLANE('',#2018);
#240=PLANE('',#2019);
#241=PLANE('',#2027);
#242=PLANE('',#2028);
#243=PLANE('',#2030);
#244=PLANE('',#2031);
#245=PLANE('',#2032);
#246=PLANE('',#2033);
#247=PLANE('',#2034);
#248=PLANE('',#2035);
#249=PLANE('',#2036);
#250=PLANE('',#2037);
#251=PLANE('',#2038);
#252=PLANE('',#2040);
#253=PLANE('',#2048);
#254=PLANE('',#2064);
#255=PLANE('',#2069);
#256=PLANE('',#2075);
#257=PLANE('',#2076);
#258=PLANE('',#2092);
#259=PLANE('',#2095);
#260=PLANE('',#2107);
#261=PLANE('',#2116);
#262=PLANE('',#2147);
#263=PLANE('',#2152);
#264=PLANE('',#2157);
#265=PLANE('',#2163);
#266=PLANE('',#2168);
#267=PLANE('',#2177);
#268=PLANE('',#2181);
#269=PLANE('',#2182);
#270=PLANE('',#2184);
#271=PLANE('',#2189);
#272=PLANE('',#2192);
#273=PLANE('',#2197);
#274=PLANE('',#2212);
#275=PLANE('',#2213);
#276=FACE_OUTER_BOUND('',#389,.T.);
#277=FACE_OUTER_BOUND('',#390,.T.);
#278=FACE_OUTER_BOUND('',#391,.T.);
#279=FACE_OUTER_BOUND('',#392,.T.);
#280=FACE_OUTER_BOUND('',#393,.T.);
#281=FACE_OUTER_BOUND('',#394,.T.);
#282=FACE_OUTER_BOUND('',#395,.T.);
#283=FACE_OUTER_BOUND('',#397,.T.);
#284=FACE_OUTER_BOUND('',#398,.T.);
#285=FACE_OUTER_BOUND('',#399,.T.);
#286=FACE_OUTER_BOUND('',#400,.T.);
#287=FACE_OUTER_BOUND('',#402,.T.);
#288=FACE_OUTER_BOUND('',#404,.T.);
#289=FACE_OUTER_BOUND('',#405,.T.);
#290=FACE_OUTER_BOUND('',#406,.T.);
#291=FACE_OUTER_BOUND('',#407,.T.);
#292=FACE_OUTER_BOUND('',#409,.T.);
#293=FACE_OUTER_BOUND('',#410,.T.);
#294=FACE_OUTER_BOUND('',#411,.T.);
#295=FACE_OUTER_BOUND('',#412,.T.);
#296=FACE_OUTER_BOUND('',#413,.T.);
#297=FACE_OUTER_BOUND('',#420,.T.);
#298=FACE_OUTER_BOUND('',#425,.T.);
#299=FACE_OUTER_BOUND('',#426,.T.);
#300=FACE_OUTER_BOUND('',#427,.T.);
#301=FACE_OUTER_BOUND('',#429,.T.);
#302=FACE_OUTER_BOUND('',#430,.T.);
#303=FACE_OUTER_BOUND('',#431,.T.);
#304=FACE_OUTER_BOUND('',#432,.T.);
#305=FACE_OUTER_BOUND('',#434,.T.);
#306=FACE_OUTER_BOUND('',#435,.T.);
#307=FACE_OUTER_BOUND('',#436,.T.);
#308=FACE_OUTER_BOUND('',#438,.T.);
#309=FACE_OUTER_BOUND('',#440,.T.);
#310=FACE_OUTER_BOUND('',#441,.T.);
#311=FACE_OUTER_BOUND('',#442,.T.);
#312=FACE_OUTER_BOUND('',#444,.T.);
#313=FACE_OUTER_BOUND('',#446,.T.);
#314=FACE_OUTER_BOUND('',#447,.T.);
#315=FACE_OUTER_BOUND('',#448,.T.);
#316=FACE_OUTER_BOUND('',#449,.T.);
#317=FACE_OUTER_BOUND('',#450,.T.);
#318=FACE_OUTER_BOUND('',#451,.T.);
#319=FACE_OUTER_BOUND('',#452,.T.);
#320=FACE_OUTER_BOUND('',#453,.T.);
#321=FACE_OUTER_BOUND('',#454,.T.);
#322=FACE_OUTER_BOUND('',#455,.T.);
#323=FACE_OUTER_BOUND('',#456,.T.);
#324=FACE_OUTER_BOUND('',#457,.T.);
#325=FACE_OUTER_BOUND('',#458,.T.);
#326=FACE_OUTER_BOUND('',#459,.T.);
#327=FACE_OUTER_BOUND('',#461,.T.);
#328=FACE_OUTER_BOUND('',#462,.T.);
#329=FACE_OUTER_BOUND('',#463,.T.);
#330=FACE_OUTER_BOUND('',#464,.T.);
#331=FACE_OUTER_BOUND('',#466,.T.);
#332=FACE_OUTER_BOUND('',#467,.T.);
#333=FACE_OUTER_BOUND('',#469,.T.);
#334=FACE_OUTER_BOUND('',#470,.T.);
#335=FACE_OUTER_BOUND('',#471,.T.);
#336=FACE_OUTER_BOUND('',#473,.T.);
#337=FACE_OUTER_BOUND('',#475,.T.);
#338=FACE_OUTER_BOUND('',#476,.T.);
#339=FACE_OUTER_BOUND('',#477,.T.);
#340=FACE_OUTER_BOUND('',#478,.T.);
#341=FACE_OUTER_BOUND('',#479,.T.);
#342=FACE_OUTER_BOUND('',#481,.T.);
#343=FACE_OUTER_BOUND('',#482,.T.);
#344=FACE_OUTER_BOUND('',#484,.T.);
#345=FACE_OUTER_BOUND('',#485,.T.);
#346=FACE_OUTER_BOUND('',#486,.T.);
#347=FACE_OUTER_BOUND('',#487,.T.);
#348=FACE_OUTER_BOUND('',#489,.T.);
#349=FACE_OUTER_BOUND('',#490,.T.);
#350=FACE_OUTER_BOUND('',#491,.T.);
#351=FACE_OUTER_BOUND('',#492,.T.);
#352=FACE_OUTER_BOUND('',#494,.T.);
#353=FACE_OUTER_BOUND('',#495,.T.);
#354=FACE_OUTER_BOUND('',#496,.T.);
#355=FACE_OUTER_BOUND('',#497,.T.);
#356=FACE_OUTER_BOUND('',#498,.T.);
#357=FACE_OUTER_BOUND('',#499,.T.);
#358=FACE_OUTER_BOUND('',#500,.T.);
#359=FACE_OUTER_BOUND('',#501,.T.);
#360=FACE_OUTER_BOUND('',#502,.T.);
#361=FACE_OUTER_BOUND('',#503,.T.);
#362=FACE_OUTER_BOUND('',#504,.T.);
#363=FACE_OUTER_BOUND('',#505,.T.);
#364=FACE_OUTER_BOUND('',#506,.T.);
#365=FACE_OUTER_BOUND('',#507,.T.);
#366=FACE_OUTER_BOUND('',#508,.T.);
#367=FACE_OUTER_BOUND('',#509,.T.);
#368=FACE_OUTER_BOUND('',#510,.T.);
#369=FACE_OUTER_BOUND('',#511,.T.);
#370=FACE_OUTER_BOUND('',#512,.T.);
#371=FACE_OUTER_BOUND('',#513,.T.);
#372=FACE_OUTER_BOUND('',#514,.T.);
#373=FACE_OUTER_BOUND('',#515,.T.);
#374=FACE_OUTER_BOUND('',#516,.T.);
#375=FACE_OUTER_BOUND('',#517,.T.);
#376=FACE_OUTER_BOUND('',#519,.T.);
#377=FACE_OUTER_BOUND('',#520,.T.);
#378=FACE_OUTER_BOUND('',#522,.T.);
#379=FACE_OUTER_BOUND('',#523,.T.);
#380=FACE_OUTER_BOUND('',#525,.T.);
#381=FACE_OUTER_BOUND('',#526,.T.);
#382=FACE_OUTER_BOUND('',#528,.T.);
#383=FACE_OUTER_BOUND('',#529,.T.);
#384=FACE_OUTER_BOUND('',#531,.T.);
#385=FACE_OUTER_BOUND('',#532,.T.);
#386=FACE_OUTER_BOUND('',#533,.T.);
#387=FACE_OUTER_BOUND('',#534,.T.);
#388=FACE_OUTER_BOUND('',#536,.T.);
#389=EDGE_LOOP('',(#1217,#1218,#1219,#1220));
#390=EDGE_LOOP('',(#1221,#1222,#1223,#1224));
#391=EDGE_LOOP('',(#1225,#1226,#1227,#1228));
#392=EDGE_LOOP('',(#1229,#1230,#1231,#1232));
#393=EDGE_LOOP('',(#1233,#1234,#1235,#1236));
#394=EDGE_LOOP('',(#1237,#1238,#1239,#1240));
#395=EDGE_LOOP('',(#1241,#1242,#1243,#1244));
#396=EDGE_LOOP('',(#1245));
#397=EDGE_LOOP('',(#1246,#1247,#1248,#1249));
#398=EDGE_LOOP('',(#1250,#1251,#1252,#1253));
#399=EDGE_LOOP('',(#1254,#1255,#1256,#1257));
#400=EDGE_LOOP('',(#1258,#1259,#1260,#1261));
#401=EDGE_LOOP('',(#1262));
#402=EDGE_LOOP('',(#1263,#1264,#1265,#1266));
#403=EDGE_LOOP('',(#1267));
#404=EDGE_LOOP('',(#1268,#1269,#1270,#1271));
#405=EDGE_LOOP('',(#1272,#1273,#1274,#1275));
#406=EDGE_LOOP('',(#1276,#1277,#1278,#1279));
#407=EDGE_LOOP('',(#1280,#1281,#1282,#1283));
#408=EDGE_LOOP('',(#1284));
#409=EDGE_LOOP('',(#1285,#1286,#1287,#1288));
#410=EDGE_LOOP('',(#1289,#1290,#1291,#1292));
#411=EDGE_LOOP('',(#1293,#1294,#1295,#1296));
#412=EDGE_LOOP('',(#1297,#1298,#1299,#1300));
#413=EDGE_LOOP('',(#1301,#1302,#1303,#1304));
#414=EDGE_LOOP('',(#1305,#1306,#1307,#1308));
#415=EDGE_LOOP('',(#1309,#1310,#1311,#1312));
#416=EDGE_LOOP('',(#1313));
#417=EDGE_LOOP('',(#1314));
#418=EDGE_LOOP('',(#1315));
#419=EDGE_LOOP('',(#1316));
#420=EDGE_LOOP('',(#1317,#1318,#1319,#1320));
#421=EDGE_LOOP('',(#1321));
#422=EDGE_LOOP('',(#1322));
#423=EDGE_LOOP('',(#1323));
#424=EDGE_LOOP('',(#1324));
#425=EDGE_LOOP('',(#1325,#1326,#1327,#1328));
#426=EDGE_LOOP('',(#1329));
#427=EDGE_LOOP('',(#1330));
#428=EDGE_LOOP('',(#1331));
#429=EDGE_LOOP('',(#1332,#1333,#1334,#1335));
#430=EDGE_LOOP('',(#1336));
#431=EDGE_LOOP('',(#1337,#1338,#1339,#1340));
#432=EDGE_LOOP('',(#1341));
#433=EDGE_LOOP('',(#1342));
#434=EDGE_LOOP('',(#1343,#1344,#1345,#1346));
#435=EDGE_LOOP('',(#1347,#1348,#1349,#1350));
#436=EDGE_LOOP('',(#1351));
#437=EDGE_LOOP('',(#1352));
#438=EDGE_LOOP('',(#1353));
#439=EDGE_LOOP('',(#1354));
#440=EDGE_LOOP('',(#1355,#1356,#1357,#1358));
#441=EDGE_LOOP('',(#1359,#1360,#1361,#1362));
#442=EDGE_LOOP('',(#1363));
#443=EDGE_LOOP('',(#1364));
#444=EDGE_LOOP('',(#1365));
#445=EDGE_LOOP('',(#1366));
#446=EDGE_LOOP('',(#1367,#1368,#1369,#1370));
#447=EDGE_LOOP('',(#1371,#1372,#1373,#1374));
#448=EDGE_LOOP('',(#1375,#1376,#1377,#1378));
#449=EDGE_LOOP('',(#1379,#1380,#1381,#1382));
#450=EDGE_LOOP('',(#1383,#1384,#1385,#1386));
#451=EDGE_LOOP('',(#1387,#1388,#1389,#1390));
#452=EDGE_LOOP('',(#1391,#1392,#1393,#1394,#1395,#1396));
#453=EDGE_LOOP('',(#1397,#1398,#1399,#1400,#1401,#1402));
#454=EDGE_LOOP('',(#1403));
#455=EDGE_LOOP('',(#1404));
#456=EDGE_LOOP('',(#1405,#1406,#1407,#1408));
#457=EDGE_LOOP('',(#1409,#1410,#1411,#1412));
#458=EDGE_LOOP('',(#1413,#1414,#1415,#1416));
#459=EDGE_LOOP('',(#1417));
#460=EDGE_LOOP('',(#1418));
#461=EDGE_LOOP('',(#1419,#1420,#1421,#1422));
#462=EDGE_LOOP('',(#1423,#1424,#1425,#1426));
#463=EDGE_LOOP('',(#1427,#1428,#1429,#1430));
#464=EDGE_LOOP('',(#1431));
#465=EDGE_LOOP('',(#1432));
#466=EDGE_LOOP('',(#1433,#1434,#1435,#1436));
#467=EDGE_LOOP('',(#1437));
#468=EDGE_LOOP('',(#1438));
#469=EDGE_LOOP('',(#1439,#1440,#1441,#1442));
#470=EDGE_LOOP('',(#1443,#1444,#1445,#1446));
#471=EDGE_LOOP('',(#1447));
#472=EDGE_LOOP('',(#1448));
#473=EDGE_LOOP('',(#1449));
#474=EDGE_LOOP('',(#1450));
#475=EDGE_LOOP('',(#1451,#1452,#1453,#1454,#1455,#1456));
#476=EDGE_LOOP('',(#1457,#1458,#1459,#1460,#1461));
#477=EDGE_LOOP('',(#1462,#1463,#1464,#1465));
#478=EDGE_LOOP('',(#1466,#1467,#1468,#1469));
#479=EDGE_LOOP('',(#1470));
#480=EDGE_LOOP('',(#1471));
#481=EDGE_LOOP('',(#1472,#1473,#1474,#1475,#1476));
#482=EDGE_LOOP('',(#1477));
#483=EDGE_LOOP('',(#1478));
#484=EDGE_LOOP('',(#1479,#1480,#1481,#1482));
#485=EDGE_LOOP('',(#1483,#1484,#1485,#1486,#1487,#1488));
#486=EDGE_LOOP('',(#1489,#1490,#1491,#1492,#1493));
#487=EDGE_LOOP('',(#1494));
#488=EDGE_LOOP('',(#1495));
#489=EDGE_LOOP('',(#1496,#1497,#1498,#1499));
#490=EDGE_LOOP('',(#1500,#1501,#1502,#1503));
#491=EDGE_LOOP('',(#1504,#1505,#1506,#1507));
#492=EDGE_LOOP('',(#1508));
#493=EDGE_LOOP('',(#1509));
#494=EDGE_LOOP('',(#1510,#1511,#1512,#1513,#1514));
#495=EDGE_LOOP('',(#1515,#1516));
#496=EDGE_LOOP('',(#1517,#1518));
#497=EDGE_LOOP('',(#1519,#1520));
#498=EDGE_LOOP('',(#1521,#1522));
#499=EDGE_LOOP('',(#1523,#1524));
#500=EDGE_LOOP('',(#1525,#1526));
#501=EDGE_LOOP('',(#1527,#1528));
#502=EDGE_LOOP('',(#1529,#1530,#1531,#1532));
#503=EDGE_LOOP('',(#1533,#1534,#1535,#1536,#1537,#1538,#1539,#1540,#1541,
#1542,#1543,#1544,#1545,#1546,#1547,#1548,#1549,#1550));
#504=EDGE_LOOP('',(#1551,#1552,#1553,#1554));
#505=EDGE_LOOP('',(#1555,#1556,#1557,#1558));
#506=EDGE_LOOP('',(#1559,#1560,#1561,#1562));
#507=EDGE_LOOP('',(#1563,#1564,#1565,#1566));
#508=EDGE_LOOP('',(#1567,#1568,#1569,#1570,#1571,#1572));
#509=EDGE_LOOP('',(#1573,#1574,#1575,#1576));
#510=EDGE_LOOP('',(#1577,#1578,#1579,#1580));
#511=EDGE_LOOP('',(#1581,#1582,#1583,#1584));
#512=EDGE_LOOP('',(#1585,#1586,#1587,#1588));
#513=EDGE_LOOP('',(#1589,#1590,#1591,#1592));
#514=EDGE_LOOP('',(#1593,#1594,#1595,#1596,#1597,#1598,#1599,#1600,#1601,
#1602,#1603,#1604,#1605,#1606,#1607,#1608,#1609,#1610));
#515=EDGE_LOOP('',(#1611,#1612,#1613,#1614));
#516=EDGE_LOOP('',(#1615,#1616,#1617,#1618));
#517=EDGE_LOOP('',(#1619));
#518=EDGE_LOOP('',(#1620));
#519=EDGE_LOOP('',(#1621,#1622,#1623,#1624));
#520=EDGE_LOOP('',(#1625));
#521=EDGE_LOOP('',(#1626));
#522=EDGE_LOOP('',(#1627,#1628,#1629,#1630));
#523=EDGE_LOOP('',(#1631));
#524=EDGE_LOOP('',(#1632));
#525=EDGE_LOOP('',(#1633,#1634,#1635,#1636));
#526=EDGE_LOOP('',(#1637));
#527=EDGE_LOOP('',(#1638));
#528=EDGE_LOOP('',(#1639,#1640,#1641,#1642));
#529=EDGE_LOOP('',(#1643));
#530=EDGE_LOOP('',(#1644));
#531=EDGE_LOOP('',(#1645,#1646,#1647,#1648));
#532=EDGE_LOOP('',(#1649,#1650,#1651,#1652));
#533=EDGE_LOOP('',(#1653,#1654,#1655,#1656));
#534=EDGE_LOOP('',(#1657));
#535=EDGE_LOOP('',(#1658));
#536=EDGE_LOOP('',(#1659));
#537=EDGE_LOOP('',(#1660));
#538=LINE('',#2844,#632);
#539=LINE('',#2850,#633);
#540=LINE('',#2856,#634);
#541=LINE('',#2862,#635);
#542=LINE('',#2868,#636);
#543=LINE('',#2874,#637);
#544=LINE('',#2879,#638);
#545=LINE('',#2881,#639);
#546=LINE('',#2883,#640);
#547=LINE('',#2884,#641);
#548=LINE('',#2887,#642);
#549=LINE('',#2889,#643);
#550=LINE('',#2890,#644);
#551=LINE('',#2893,#645);
#552=LINE('',#2895,#646);
#553=LINE('',#2896,#647);
#554=LINE('',#2898,#648);
#555=LINE('',#2900,#649);
#556=LINE('',#2904,#650);
#557=LINE('',#2906,#651);
#558=LINE('',#2908,#652);
#559=LINE('',#2909,#653);
#560=LINE('',#2912,#654);
#561=LINE('',#2914,#655);
#562=LINE('',#2915,#656);
#563=LINE('',#2918,#657);
#564=LINE('',#2920,#658);
#565=LINE('',#2921,#659);
#566=LINE('',#2923,#660);
#567=LINE('',#2925,#661);
#568=LINE('',#2929,#662);
#569=LINE('',#2931,#663);
#570=LINE('',#2933,#664);
#571=LINE('',#2934,#665);
#572=LINE('',#2937,#666);
#573=LINE('',#2939,#667);
#574=LINE('',#2940,#668);
#575=LINE('',#2943,#669);
#576=LINE('',#2945,#670);
#577=LINE('',#2946,#671);
#578=LINE('',#2948,#672);
#579=LINE('',#2949,#673);
#580=LINE('',#2957,#674);
#581=LINE('',#2967,#675);
#582=LINE('',#2973,#676);
#583=LINE('',#2980,#677);
#584=LINE('',#2986,#678);
#585=LINE('',#2995,#679);
#586=LINE('',#3001,#680);
#587=LINE('',#3009,#681);
#588=LINE('',#3011,#682);
#589=LINE('',#3013,#683);
#590=LINE('',#3014,#684);
#591=LINE('',#3017,#685);
#592=LINE('',#3019,#686);
#593=LINE('',#3020,#687);
#594=LINE('',#3023,#688);
#595=LINE('',#3025,#689);
#596=LINE('',#3026,#690);
#597=LINE('',#3029,#691);
#598=LINE('',#3031,#692);
#599=LINE('',#3032,#693);
#600=LINE('',#3035,#694);
#601=LINE('',#3037,#695);
#602=LINE('',#3038,#696);
#603=LINE('',#3040,#697);
#604=LINE('',#3041,#698);
#605=LINE('',#3053,#699);
#606=LINE('',#3057,#700);
#607=LINE('',#3061,#701);
#608=LINE('',#3068,#702);
#609=LINE('',#3070,#703);
#610=LINE('',#3083,#704);
#611=LINE('',#3092,#705);
#612=LINE('',#3098,#706);
#613=LINE('',#3103,#707);
#614=LINE('',#3121,#708);
#615=LINE('',#3127,#709);
#616=LINE('',#3131,#710);
#617=LINE('',#3137,#711);
#618=LINE('',#3142,#712);
#619=LINE('',#3157,#713);
#620=LINE('',#3166,#714);
#621=LINE('',#3170,#715);
#622=LINE('',#3174,#716);
#623=LINE('',#3177,#717);
#624=LINE('',#3313,#718);
#625=LINE('',#3566,#719);
#626=LINE('',#3608,#720);
#627=LINE('',#3613,#721);
#628=LINE('',#3622,#722);
#629=LINE('',#3627,#723);
#630=LINE('',#3638,#724);
#631=LINE('',#3644,#725);
#632=VECTOR('',#2231,0.275);
#633=VECTOR('',#2238,0.275);
#634=VECTOR('',#2245,0.275);
#635=VECTOR('',#2252,0.275);
#636=VECTOR('',#2259,0.6);
#637=VECTOR('',#2266,0.6);
#638=VECTOR('',#2271,1.);
#639=VECTOR('',#2272,1.);
#640=VECTOR('',#2273,1.);
#641=VECTOR('',#2274,1.);
#642=VECTOR('',#2277,1.);
#643=VECTOR('',#2278,1.);
#644=VECTOR('',#2279,1.);
#645=VECTOR('',#2282,1.);
#646=VECTOR('',#2283,1.);
#647=VECTOR('',#2284,1.);
#648=VECTOR('',#2287,1.);
#649=VECTOR('',#2290,1.);
#650=VECTOR('',#2293,1.);
#651=VECTOR('',#2294,1.);
#652=VECTOR('',#2295,1.);
#653=VECTOR('',#2296,1.);
#654=VECTOR('',#2299,1.);
#655=VECTOR('',#2300,1.);
#656=VECTOR('',#2301,1.);
#657=VECTOR('',#2304,1.);
#658=VECTOR('',#2305,1.);
#659=VECTOR('',#2306,1.);
#660=VECTOR('',#2309,1.);
#661=VECTOR('',#2312,1.);
#662=VECTOR('',#2315,1.);
#663=VECTOR('',#2316,1.);
#664=VECTOR('',#2317,1.);
#665=VECTOR('',#2318,1.);
#666=VECTOR('',#2321,1.);
#667=VECTOR('',#2322,1.);
#668=VECTOR('',#2323,1.);
#669=VECTOR('',#2326,1.);
#670=VECTOR('',#2327,1.);
#671=VECTOR('',#2328,1.);
#672=VECTOR('',#2331,1.);
#673=VECTOR('',#2332,1.);
#674=VECTOR('',#2343,0.165);
#675=VECTOR('',#2356,0.9);
#676=VECTOR('',#2365,0.6);
#677=VECTOR('',#2374,0.605);
#678=VECTOR('',#2381,0.8);
#679=VECTOR('',#2394,0.225);
#680=VECTOR('',#2401,0.8);
#681=VECTOR('',#2412,1.);
#682=VECTOR('',#2413,1.);
#683=VECTOR('',#2414,1.);
#684=VECTOR('',#2415,1.);
#685=VECTOR('',#2418,1.);
#686=VECTOR('',#2419,1.);
#687=VECTOR('',#2420,1.);
#688=VECTOR('',#2423,1.);
#689=VECTOR('',#2424,1.);
#690=VECTOR('',#2425,1.);
#691=VECTOR('',#2428,1.);
#692=VECTOR('',#2429,1.);
#693=VECTOR('',#2430,1.);
#694=VECTOR('',#2433,1.);
#695=VECTOR('',#2434,1.);
#696=VECTOR('',#2435,1.);
#697=VECTOR('',#2438,1.);
#698=VECTOR('',#2439,1.);
#699=VECTOR('',#2456,0.325);
#700=VECTOR('',#2461,0.35);
#701=VECTOR('',#2466,0.335);
#702=VECTOR('',#2475,0.21);
#703=VECTOR('',#2478,0.2);
#704=VECTOR('',#2499,1.6);
#705=VECTOR('',#2510,1.6);
#706=VECTOR('',#2519,0.62);
#707=VECTOR('',#2524,2.5);
#708=VECTOR('',#2549,1.070235);
#709=VECTOR('',#2556,0.6);
#710=VECTOR('',#2561,0.63);
#711=VECTOR('',#2570,1.070235);
#712=VECTOR('',#2577,0.63);
#713=VECTOR('',#2596,1.129765);
#714=VECTOR('',#2607,1.57);
#715=VECTOR('',#2612,1.6);
#716=VECTOR('',#2617,1.57);
#717=VECTOR('',#2622,1.129765);
#718=VECTOR('',#2669,1.123812);
#719=VECTOR('',#2738,1.076188);
#720=VECTOR('',#2767,1.119765);
#721=VECTOR('',#2774,1.085235);
#722=VECTOR('',#2785,1.119765);
#723=VECTOR('',#2792,1.085235);
#724=VECTOR('',#2809,1.2);
#725=VECTOR('',#2816,1.6);
#726=CIRCLE('',#1964,0.275);
#727=CIRCLE('',#1965,0.275);
#728=CIRCLE('',#1967,0.275);
#729=CIRCLE('',#1968,0.275);
#730=CIRCLE('',#1970,0.275);
#731=CIRCLE('',#1971,0.275);
#732=CIRCLE('',#1973,0.275);
#733=CIRCLE('',#1974,0.275);
#734=CIRCLE('',#1976,0.6);
#735=CIRCLE('',#1977,0.6);
#736=CIRCLE('',#1979,0.6);
#737=CIRCLE('',#1980,0.6);
#738=CIRCLE('',#1999,0.165);
#739=CIRCLE('',#2000,0.165);
#740=CIRCLE('',#2003,0.9);
#741=CIRCLE('',#2004,0.6);
#742=CIRCLE('',#2006,0.9);
#743=CIRCLE('',#2009,0.6);
#744=CIRCLE('',#2013,0.605);
#745=CIRCLE('',#2014,0.605);
#746=CIRCLE('',#2016,0.8);
#747=CIRCLE('',#2017,0.8);
#748=CIRCLE('',#2022,0.225);
#749=CIRCLE('',#2023,0.225);
#750=CIRCLE('',#2025,0.8);
#751=CIRCLE('',#2026,0.8);
#752=CIRCLE('',#2039,0.1954);
#753=CIRCLE('',#2041,0.3);
#754=CIRCLE('',#2043,0.35);
#755=CIRCLE('',#2045,0.35);
#756=CIRCLE('',#2047,0.32);
#757=CIRCLE('',#2049,0.22);
#758=CIRCLE('',#2051,0.1954);
#759=CIRCLE('',#2062,1.6);
#760=CIRCLE('',#2063,1.6);
#761=CIRCLE('',#2065,0.62);
#762=CIRCLE('',#2067,1.6);
#763=CIRCLE('',#2068,1.6);
#764=CIRCLE('',#2070,0.62);
#765=CIRCLE('',#2073,2.5);
#766=CIRCLE('',#2074,2.5);
#767=CIRCLE('',#2080,1.070235);
#768=CIRCLE('',#2081,1.070235);
#769=CIRCLE('',#2082,0.309556);
#770=CIRCLE('',#2083,1.070235);
#771=CIRCLE('',#2084,1.070235);
#772=CIRCLE('',#2086,1.070235);
#773=CIRCLE('',#2088,0.6);
#774=CIRCLE('',#2089,0.6);
#775=CIRCLE('',#2091,0.66);
#776=CIRCLE('',#2094,1.070235);
#777=CIRCLE('',#2096,0.66);
#778=CIRCLE('',#2100,1.129765);
#779=CIRCLE('',#2101,1.129765);
#780=CIRCLE('',#2102,0.309556);
#781=CIRCLE('',#2103,1.129765);
#782=CIRCLE('',#2104,1.129765);
#783=CIRCLE('',#2106,1.129765);
#784=CIRCLE('',#2108,1.54);
#785=CIRCLE('',#2109,1.129765);
#786=CIRCLE('',#2111,1.6);
#787=CIRCLE('',#2113,1.6);
#788=CIRCLE('',#2115,1.54);
#789=CIRCLE('',#2120,0.29765);
#790=CIRCLE('',#2122,0.29765);
#791=CIRCLE('',#2124,0.29765);
#792=CIRCLE('',#2126,0.29765);
#793=CIRCLE('',#2128,0.29765);
#794=CIRCLE('',#2130,0.29765);
#795=CIRCLE('',#2132,0.29765);
#796=CIRCLE('',#2135,0.303778037777585);
#797=CIRCLE('',#2136,0.303778037777585);
#798=CIRCLE('',#2138,1.123812);
#799=CIRCLE('',#2139,1.123812);
#800=CIRCLE('',#2140,1.123812);
#801=CIRCLE('',#2141,1.123812);
#802=CIRCLE('',#2142,1.123812);
#803=CIRCLE('',#2143,1.123812);
#804=CIRCLE('',#2144,1.123812);
#805=CIRCLE('',#2145,1.123812);
#806=CIRCLE('',#2146,1.123812);
#807=CIRCLE('',#2148,1.076188);
#808=CIRCLE('',#2149,0.303778037777585);
#809=CIRCLE('',#2151,0.303778037777585);
#810=CIRCLE('',#2153,1.076188);
#811=CIRCLE('',#2154,0.303778037777585);
#812=CIRCLE('',#2156,0.303778037777585);
#813=CIRCLE('',#2158,1.076188);
#814=CIRCLE('',#2159,1.076188);
#815=CIRCLE('',#2160,0.303778037777585);
#816=CIRCLE('',#2162,0.303778037777585);
#817=CIRCLE('',#2164,1.076188);
#818=CIRCLE('',#2165,0.303778037777585);
#819=CIRCLE('',#2167,0.303778037777585);
#820=CIRCLE('',#2169,1.076188);
#821=CIRCLE('',#2170,0.303778037777585);
#822=CIRCLE('',#2172,0.303778037777585);
#823=CIRCLE('',#2174,1.076188);
#824=CIRCLE('',#2175,1.076188);
#825=CIRCLE('',#2176,1.076188);
#826=CIRCLE('',#2178,0.303778037777585);
#827=CIRCLE('',#2180,0.303778037777585);
#828=CIRCLE('',#2185,1.119765);
#829=CIRCLE('',#2186,1.085235);
#830=CIRCLE('',#2188,1.119765);
#831=CIRCLE('',#2190,1.085235);
#832=CIRCLE('',#2193,1.119765);
#833=CIRCLE('',#2194,1.085235);
#834=CIRCLE('',#2196,1.119765);
#835=CIRCLE('',#2198,1.085235);
#836=CIRCLE('',#2207,1.2);
#837=CIRCLE('',#2208,1.2);
#838=CIRCLE('',#2210,1.6);
#839=CIRCLE('',#2211,1.6);
#840=VERTEX_POINT('',#2841);
#841=VERTEX_POINT('',#2843);
#842=VERTEX_POINT('',#2847);
#843=VERTEX_POINT('',#2849);
#844=VERTEX_POINT('',#2853);
#845=VERTEX_POINT('',#2855);
#846=VERTEX_POINT('',#2859);
#847=VERTEX_POINT('',#2861);
#848=VERTEX_POINT('',#2865);
#849=VERTEX_POINT('',#2867);
#850=VERTEX_POINT('',#2871);
#851=VERTEX_POINT('',#2873);
#852=VERTEX_POINT('',#2877);
#853=VERTEX_POINT('',#2878);
#854=VERTEX_POINT('',#2880);
#855=VERTEX_POINT('',#2882);
#856=VERTEX_POINT('',#2886);
#857=VERTEX_POINT('',#2888);
#858=VERTEX_POINT('',#2892);
#859=VERTEX_POINT('',#2894);
#860=VERTEX_POINT('',#2902);
#861=VERTEX_POINT('',#2903);
#862=VERTEX_POINT('',#2905);
#863=VERTEX_POINT('',#2907);
#864=VERTEX_POINT('',#2911);
#865=VERTEX_POINT('',#2913);
#866=VERTEX_POINT('',#2917);
#867=VERTEX_POINT('',#2919);
#868=VERTEX_POINT('',#2927);
#869=VERTEX_POINT('',#2928);
#870=VERTEX_POINT('',#2930);
#871=VERTEX_POINT('',#2932);
#872=VERTEX_POINT('',#2936);
#873=VERTEX_POINT('',#2938);
#874=VERTEX_POINT('',#2942);
#875=VERTEX_POINT('',#2944);
#876=VERTEX_POINT('',#2954);
#877=VERTEX_POINT('',#2956);
#878=VERTEX_POINT('',#2961);
#879=VERTEX_POINT('',#2963);
#880=VERTEX_POINT('',#2966);
#881=VERTEX_POINT('',#2971);
#882=VERTEX_POINT('',#2977);
#883=VERTEX_POINT('',#2979);
#884=VERTEX_POINT('',#2983);
#885=VERTEX_POINT('',#2985);
#886=VERTEX_POINT('',#2992);
#887=VERTEX_POINT('',#2994);
#888=VERTEX_POINT('',#2998);
#889=VERTEX_POINT('',#3000);
#890=VERTEX_POINT('',#3007);
#891=VERTEX_POINT('',#3008);
#892=VERTEX_POINT('',#3010);
#893=VERTEX_POINT('',#3012);
#894=VERTEX_POINT('',#3016);
#895=VERTEX_POINT('',#3018);
#896=VERTEX_POINT('',#3022);
#897=VERTEX_POINT('',#3024);
#898=VERTEX_POINT('',#3028);
#899=VERTEX_POINT('',#3030);
#900=VERTEX_POINT('',#3034);
#901=VERTEX_POINT('',#3036);
#902=VERTEX_POINT('',#3045);
#903=VERTEX_POINT('',#3048);
#904=VERTEX_POINT('',#3051);
#905=VERTEX_POINT('',#3055);
#906=VERTEX_POINT('',#3059);
#907=VERTEX_POINT('',#3063);
#908=VERTEX_POINT('',#3066);
#909=VERTEX_POINT('',#3080);
#910=VERTEX_POINT('',#3082);
#911=VERTEX_POINT('',#3086);
#912=VERTEX_POINT('',#3089);
#913=VERTEX_POINT('',#3091);
#914=VERTEX_POINT('',#3095);
#915=VERTEX_POINT('',#3100);
#916=VERTEX_POINT('',#3102);
#917=VERTEX_POINT('',#3110);
#918=VERTEX_POINT('',#3111);
#919=VERTEX_POINT('',#3114);
#920=VERTEX_POINT('',#3116);
#921=VERTEX_POINT('',#3120);
#922=VERTEX_POINT('',#3124);
#923=VERTEX_POINT('',#3126);
#924=VERTEX_POINT('',#3130);
#925=VERTEX_POINT('',#3135);
#926=VERTEX_POINT('',#3139);
#927=VERTEX_POINT('',#3145);
#928=VERTEX_POINT('',#3146);
#929=VERTEX_POINT('',#3149);
#930=VERTEX_POINT('',#3151);
#931=VERTEX_POINT('',#3155);
#932=VERTEX_POINT('',#3159);
#933=VERTEX_POINT('',#3161);
#934=VERTEX_POINT('',#3164);
#935=VERTEX_POINT('',#3168);
#936=VERTEX_POINT('',#3172);
#937=VERTEX_POINT('',#3180);
#938=VERTEX_POINT('',#3181);
#939=VERTEX_POINT('',#3184);
#940=VERTEX_POINT('',#3185);
#941=VERTEX_POINT('',#3188);
#942=VERTEX_POINT('',#3189);
#943=VERTEX_POINT('',#3192);
#944=VERTEX_POINT('',#3193);
#945=VERTEX_POINT('',#3196);
#946=VERTEX_POINT('',#3197);
#947=VERTEX_POINT('',#3200);
#948=VERTEX_POINT('',#3201);
#949=VERTEX_POINT('',#3204);
#950=VERTEX_POINT('',#3205);
#951=VERTEX_POINT('',#3209);
#952=VERTEX_POINT('',#3210);
#953=VERTEX_POINT('',#3233);
#954=VERTEX_POINT('',#3235);
#955=VERTEX_POINT('',#3260);
#956=VERTEX_POINT('',#3262);
#957=VERTEX_POINT('',#3285);
#958=VERTEX_POINT('',#3287);
#959=VERTEX_POINT('',#3310);
#960=VERTEX_POINT('',#3312);
#961=VERTEX_POINT('',#3315);
#962=VERTEX_POINT('',#3317);
#963=VERTEX_POINT('',#3340);
#964=VERTEX_POINT('',#3342);
#965=VERTEX_POINT('',#3365);
#966=VERTEX_POINT('',#3367);
#967=VERTEX_POINT('',#3390);
#968=VERTEX_POINT('',#3392);
#969=VERTEX_POINT('',#3417);
#970=VERTEX_POINT('',#3421);
#971=VERTEX_POINT('',#3446);
#972=VERTEX_POINT('',#3450);
#973=VERTEX_POINT('',#3475);
#974=VERTEX_POINT('',#3477);
#975=VERTEX_POINT('',#3481);
#976=VERTEX_POINT('',#3506);
#977=VERTEX_POINT('',#3510);
#978=VERTEX_POINT('',#3535);
#979=VERTEX_POINT('',#3539);
#980=VERTEX_POINT('',#3564);
#981=VERTEX_POINT('',#3567);
#982=VERTEX_POINT('',#3569);
#983=VERTEX_POINT('',#3601);
#984=VERTEX_POINT('',#3603);
#985=VERTEX_POINT('',#3606);
#986=VERTEX_POINT('',#3610);
#987=VERTEX_POINT('',#3615);
#988=VERTEX_POINT('',#3617);
#989=VERTEX_POINT('',#3620);
#990=VERTEX_POINT('',#3624);
#991=VERTEX_POINT('',#3635);
#992=VERTEX_POINT('',#3637);
#993=VERTEX_POINT('',#3641);
#994=VERTEX_POINT('',#3643);
#995=EDGE_CURVE('',#840,#840,#726,.T.);
#996=EDGE_CURVE('',#840,#841,#538,.T.);
#997=EDGE_CURVE('',#841,#841,#727,.T.);
#998=EDGE_CURVE('',#842,#842,#728,.T.);
#999=EDGE_CURVE('',#842,#843,#539,.T.);
#1000=EDGE_CURVE('',#843,#843,#729,.T.);
#1001=EDGE_CURVE('',#844,#844,#730,.T.);
#1002=EDGE_CURVE('',#844,#845,#540,.T.);
#1003=EDGE_CURVE('',#845,#845,#731,.T.);
#1004=EDGE_CURVE('',#846,#846,#732,.T.);
#1005=EDGE_CURVE('',#846,#847,#541,.T.);
#1006=EDGE_CURVE('',#847,#847,#733,.T.);
#1007=EDGE_CURVE('',#848,#848,#734,.T.);
#1008=EDGE_CURVE('',#848,#849,#542,.T.);
#1009=EDGE_CURVE('',#849,#849,#735,.T.);
#1010=EDGE_CURVE('',#850,#850,#736,.T.);
#1011=EDGE_CURVE('',#850,#851,#543,.T.);
#1012=EDGE_CURVE('',#851,#851,#737,.T.);
#1013=EDGE_CURVE('',#852,#853,#544,.T.);
#1014=EDGE_CURVE('',#852,#854,#545,.T.);
#1015=EDGE_CURVE('',#854,#855,#546,.T.);
#1016=EDGE_CURVE('',#855,#853,#547,.T.);
#1017=EDGE_CURVE('',#856,#852,#548,.T.);
#1018=EDGE_CURVE('',#857,#856,#549,.T.);
#1019=EDGE_CURVE('',#854,#857,#550,.T.);
#1020=EDGE_CURVE('',#853,#858,#551,.T.);
#1021=EDGE_CURVE('',#855,#859,#552,.T.);
#1022=EDGE_CURVE('',#858,#859,#553,.T.);
#1023=EDGE_CURVE('',#859,#857,#554,.T.);
#1024=EDGE_CURVE('',#858,#856,#555,.T.);
#1025=EDGE_CURVE('',#860,#861,#556,.T.);
#1026=EDGE_CURVE('',#860,#862,#557,.T.);
#1027=EDGE_CURVE('',#862,#863,#558,.T.);
#1028=EDGE_CURVE('',#863,#861,#559,.T.);
#1029=EDGE_CURVE('',#864,#860,#560,.T.);
#1030=EDGE_CURVE('',#865,#864,#561,.T.);
#1031=EDGE_CURVE('',#862,#865,#562,.T.);
#1032=EDGE_CURVE('',#861,#866,#563,.T.);
#1033=EDGE_CURVE('',#863,#867,#564,.T.);
#1034=EDGE_CURVE('',#866,#867,#565,.T.);
#1035=EDGE_CURVE('',#867,#865,#566,.T.);
#1036=EDGE_CURVE('',#866,#864,#567,.T.);
#1037=EDGE_CURVE('',#868,#869,#568,.T.);
#1038=EDGE_CURVE('',#869,#870,#569,.T.);
#1039=EDGE_CURVE('',#871,#870,#570,.T.);
#1040=EDGE_CURVE('',#868,#871,#571,.T.);
#1041=EDGE_CURVE('',#872,#868,#572,.T.);
#1042=EDGE_CURVE('',#873,#871,#573,.T.);
#1043=EDGE_CURVE('',#872,#873,#574,.T.);
#1044=EDGE_CURVE('',#874,#872,#575,.T.);
#1045=EDGE_CURVE('',#875,#873,#576,.T.);
#1046=EDGE_CURVE('',#874,#875,#577,.T.);
#1047=EDGE_CURVE('',#869,#874,#578,.T.);
#1048=EDGE_CURVE('',#870,#875,#579,.T.);
#1049=EDGE_CURVE('',#876,#876,#738,.T.);
#1050=EDGE_CURVE('',#876,#877,#580,.T.);
#1051=EDGE_CURVE('',#877,#877,#739,.T.);
#1052=EDGE_CURVE('',#878,#878,#740,.T.);
#1053=EDGE_CURVE('',#879,#879,#741,.T.);
#1054=EDGE_CURVE('',#878,#880,#581,.T.);
#1055=EDGE_CURVE('',#880,#880,#742,.T.);
#1056=EDGE_CURVE('',#881,#881,#743,.T.);
#1057=EDGE_CURVE('',#881,#879,#582,.T.);
#1058=EDGE_CURVE('',#882,#882,#744,.T.);
#1059=EDGE_CURVE('',#882,#883,#583,.T.);
#1060=EDGE_CURVE('',#883,#883,#745,.T.);
#1061=EDGE_CURVE('',#884,#884,#746,.T.);
#1062=EDGE_CURVE('',#884,#885,#584,.T.);
#1063=EDGE_CURVE('',#885,#885,#747,.T.);
#1064=EDGE_CURVE('',#886,#886,#748,.T.);
#1065=EDGE_CURVE('',#886,#887,#585,.T.);
#1066=EDGE_CURVE('',#887,#887,#749,.T.);
#1067=EDGE_CURVE('',#888,#888,#750,.T.);
#1068=EDGE_CURVE('',#888,#889,#586,.T.);
#1069=EDGE_CURVE('',#889,#889,#751,.T.);
#1070=EDGE_CURVE('',#890,#891,#587,.T.);
#1071=EDGE_CURVE('',#891,#892,#588,.T.);
#1072=EDGE_CURVE('',#892,#893,#589,.T.);
#1073=EDGE_CURVE('',#890,#893,#590,.T.);
#1074=EDGE_CURVE('',#891,#894,#591,.T.);
#1075=EDGE_CURVE('',#894,#895,#592,.T.);
#1076=EDGE_CURVE('',#895,#892,#593,.T.);
#1077=EDGE_CURVE('',#894,#896,#594,.T.);
#1078=EDGE_CURVE('',#896,#897,#595,.T.);
#1079=EDGE_CURVE('',#897,#895,#596,.T.);
#1080=EDGE_CURVE('',#896,#898,#597,.T.);
#1081=EDGE_CURVE('',#898,#899,#598,.T.);
#1082=EDGE_CURVE('',#899,#897,#599,.T.);
#1083=EDGE_CURVE('',#898,#900,#600,.T.);
#1084=EDGE_CURVE('',#900,#901,#601,.T.);
#1085=EDGE_CURVE('',#901,#899,#602,.T.);
#1086=EDGE_CURVE('',#900,#890,#603,.T.);
#1087=EDGE_CURVE('',#893,#901,#604,.T.);
#1088=EDGE_CURVE('',#902,#902,#752,.T.);
#1089=EDGE_CURVE('',#903,#903,#753,.T.);
#1090=EDGE_CURVE('',#904,#904,#754,.T.);
#1091=EDGE_CURVE('',#904,#903,#605,.T.);
#1092=EDGE_CURVE('',#905,#905,#755,.T.);
#1093=EDGE_CURVE('',#905,#904,#606,.T.);
#1094=EDGE_CURVE('',#906,#906,#756,.T.);
#1095=EDGE_CURVE('',#906,#905,#607,.T.);
#1096=EDGE_CURVE('',#907,#907,#757,.T.);
#1097=EDGE_CURVE('',#908,#908,#758,.F.);
#1098=EDGE_CURVE('',#908,#907,#608,.T.);
#1099=EDGE_CURVE('',#902,#908,#609,.T.);
#1100=EDGE_CURVE('',#909,#909,#759,.T.);
#1101=EDGE_CURVE('',#909,#910,#610,.T.);
#1102=EDGE_CURVE('',#910,#910,#760,.T.);
#1103=EDGE_CURVE('',#911,#911,#761,.T.);
#1104=EDGE_CURVE('',#912,#912,#762,.T.);
#1105=EDGE_CURVE('',#912,#913,#611,.T.);
#1106=EDGE_CURVE('',#913,#913,#763,.T.);
#1107=EDGE_CURVE('',#914,#914,#764,.T.);
#1108=EDGE_CURVE('',#911,#914,#612,.T.);
#1109=EDGE_CURVE('',#915,#915,#765,.T.);
#1110=EDGE_CURVE('',#915,#916,#613,.T.);
#1111=EDGE_CURVE('',#916,#916,#766,.T.);
#1112=EDGE_CURVE('',#917,#918,#767,.T.);
#1113=EDGE_CURVE('',#918,#917,#768,.T.);
#1114=EDGE_CURVE('',#918,#919,#769,.T.);
#1115=EDGE_CURVE('',#920,#919,#770,.T.);
#1116=EDGE_CURVE('',#919,#920,#771,.T.);
#1117=EDGE_CURVE('',#920,#921,#614,.T.);
#1118=EDGE_CURVE('',#921,#921,#772,.T.);
#1119=EDGE_CURVE('',#922,#922,#773,.T.);
#1120=EDGE_CURVE('',#922,#923,#615,.T.);
#1121=EDGE_CURVE('',#923,#923,#774,.T.);
#1122=EDGE_CURVE('',#923,#924,#616,.T.);
#1123=EDGE_CURVE('',#924,#924,#775,.T.);
#1124=EDGE_CURVE('',#925,#925,#776,.T.);
#1125=EDGE_CURVE('',#925,#917,#617,.T.);
#1126=EDGE_CURVE('',#926,#926,#777,.T.);
#1127=EDGE_CURVE('',#926,#922,#618,.T.);
#1128=EDGE_CURVE('',#927,#928,#778,.T.);
#1129=EDGE_CURVE('',#928,#927,#779,.T.);
#1130=EDGE_CURVE('',#928,#929,#780,.T.);
#1131=EDGE_CURVE('',#930,#929,#781,.T.);
#1132=EDGE_CURVE('',#929,#930,#782,.T.);
#1133=EDGE_CURVE('',#931,#931,#783,.T.);
#1134=EDGE_CURVE('',#931,#930,#619,.T.);
#1135=EDGE_CURVE('',#932,#932,#784,.T.);
#1136=EDGE_CURVE('',#933,#933,#785,.T.);
#1137=EDGE_CURVE('',#934,#934,#786,.T.);
#1138=EDGE_CURVE('',#934,#932,#620,.T.);
#1139=EDGE_CURVE('',#935,#935,#787,.T.);
#1140=EDGE_CURVE('',#935,#934,#621,.T.);
#1141=EDGE_CURVE('',#936,#936,#788,.T.);
#1142=EDGE_CURVE('',#936,#935,#622,.T.);
#1143=EDGE_CURVE('',#927,#933,#623,.T.);
#1144=EDGE_CURVE('',#937,#938,#789,.T.);
#1145=EDGE_CURVE('',#939,#940,#790,.T.);
#1146=EDGE_CURVE('',#941,#942,#791,.T.);
#1147=EDGE_CURVE('',#943,#944,#792,.T.);
#1148=EDGE_CURVE('',#945,#946,#793,.T.);
#1149=EDGE_CURVE('',#947,#948,#794,.T.);
#1150=EDGE_CURVE('',#949,#950,#795,.T.);
#1151=EDGE_CURVE('',#951,#952,#11,.T.);
#1152=EDGE_CURVE('',#953,#951,#796,.T.);
#1153=EDGE_CURVE('',#954,#953,#12,.T.);
#1154=EDGE_CURVE('',#952,#954,#797,.T.);
#1155=EDGE_CURVE('',#955,#953,#798,.T.);
#1156=EDGE_CURVE('',#955,#956,#13,.T.);
#1157=EDGE_CURVE('',#957,#956,#799,.T.);
#1158=EDGE_CURVE('',#957,#958,#14,.T.);
#1159=EDGE_CURVE('',#959,#958,#800,.T.);
#1160=EDGE_CURVE('',#959,#960,#624,.T.);
#1161=EDGE_CURVE('',#960,#960,#801,.T.);
#1162=EDGE_CURVE('',#961,#959,#802,.T.);
#1163=EDGE_CURVE('',#961,#962,#15,.T.);
#1164=EDGE_CURVE('',#963,#962,#803,.T.);
#1165=EDGE_CURVE('',#963,#964,#16,.T.);
#1166=EDGE_CURVE('',#965,#964,#804,.T.);
#1167=EDGE_CURVE('',#965,#966,#17,.T.);
#1168=EDGE_CURVE('',#967,#966,#805,.T.);
#1169=EDGE_CURVE('',#967,#968,#18,.T.);
#1170=EDGE_CURVE('',#954,#968,#806,.T.);
#1171=EDGE_CURVE('',#951,#969,#807,.T.);
#1172=EDGE_CURVE('',#969,#955,#808,.T.);
#1173=EDGE_CURVE('',#970,#969,#19,.T.);
#1174=EDGE_CURVE('',#956,#970,#809,.T.);
#1175=EDGE_CURVE('',#970,#971,#810,.T.);
#1176=EDGE_CURVE('',#971,#957,#811,.T.);
#1177=EDGE_CURVE('',#972,#971,#20,.T.);
#1178=EDGE_CURVE('',#958,#972,#812,.T.);
#1179=EDGE_CURVE('',#972,#973,#813,.T.);
#1180=EDGE_CURVE('',#973,#974,#814,.T.);
#1181=EDGE_CURVE('',#974,#961,#815,.T.);
#1182=EDGE_CURVE('',#975,#974,#21,.T.);
#1183=EDGE_CURVE('',#962,#975,#816,.T.);
#1184=EDGE_CURVE('',#975,#976,#817,.T.);
#1185=EDGE_CURVE('',#976,#963,#818,.T.);
#1186=EDGE_CURVE('',#977,#976,#22,.T.);
#1187=EDGE_CURVE('',#964,#977,#819,.T.);
#1188=EDGE_CURVE('',#977,#978,#820,.T.);
#1189=EDGE_CURVE('',#978,#965,#821,.T.);
#1190=EDGE_CURVE('',#979,#978,#23,.T.);
#1191=EDGE_CURVE('',#966,#979,#822,.T.);
#1192=EDGE_CURVE('',#980,#980,#823,.T.);
#1193=EDGE_CURVE('',#980,#973,#625,.T.);
#1194=EDGE_CURVE('',#981,#952,#824,.T.);
#1195=EDGE_CURVE('',#981,#982,#24,.T.);
#1196=EDGE_CURVE('',#979,#982,#825,.T.);
#1197=EDGE_CURVE('',#968,#981,#826,.T.);
#1198=EDGE_CURVE('',#982,#967,#827,.T.);
#1199=EDGE_CURVE('',#983,#983,#828,.T.);
#1200=EDGE_CURVE('',#984,#984,#829,.T.);
#1201=EDGE_CURVE('',#985,#985,#830,.T.);
#1202=EDGE_CURVE('',#985,#983,#626,.T.);
#1203=EDGE_CURVE('',#986,#986,#831,.T.);
#1204=EDGE_CURVE('',#986,#984,#627,.T.);
#1205=EDGE_CURVE('',#987,#987,#832,.T.);
#1206=EDGE_CURVE('',#988,#988,#833,.T.);
#1207=EDGE_CURVE('',#989,#989,#834,.T.);
#1208=EDGE_CURVE('',#989,#987,#628,.T.);
#1209=EDGE_CURVE('',#990,#990,#835,.T.);
#1210=EDGE_CURVE('',#990,#988,#629,.T.);
#1211=EDGE_CURVE('',#991,#991,#836,.T.);
#1212=EDGE_CURVE('',#991,#992,#630,.T.);
#1213=EDGE_CURVE('',#992,#992,#837,.T.);
#1214=EDGE_CURVE('',#993,#993,#838,.T.);
#1215=EDGE_CURVE('',#993,#994,#631,.T.);
#1216=EDGE_CURVE('',#994,#994,#839,.T.);
#1217=ORIENTED_EDGE('',*,*,#995,.F.);
#1218=ORIENTED_EDGE('',*,*,#996,.T.);
#1219=ORIENTED_EDGE('',*,*,#997,.F.);
#1220=ORIENTED_EDGE('',*,*,#996,.F.);
#1221=ORIENTED_EDGE('',*,*,#998,.F.);
#1222=ORIENTED_EDGE('',*,*,#999,.T.);
#1223=ORIENTED_EDGE('',*,*,#1000,.F.);
#1224=ORIENTED_EDGE('',*,*,#999,.F.);
#1225=ORIENTED_EDGE('',*,*,#1001,.F.);
#1226=ORIENTED_EDGE('',*,*,#1002,.T.);
#1227=ORIENTED_EDGE('',*,*,#1003,.F.);
#1228=ORIENTED_EDGE('',*,*,#1002,.F.);
#1229=ORIENTED_EDGE('',*,*,#1004,.F.);
#1230=ORIENTED_EDGE('',*,*,#1005,.T.);
#1231=ORIENTED_EDGE('',*,*,#1006,.F.);
#1232=ORIENTED_EDGE('',*,*,#1005,.F.);
#1233=ORIENTED_EDGE('',*,*,#1007,.F.);
#1234=ORIENTED_EDGE('',*,*,#1008,.T.);
#1235=ORIENTED_EDGE('',*,*,#1009,.F.);
#1236=ORIENTED_EDGE('',*,*,#1008,.F.);
#1237=ORIENTED_EDGE('',*,*,#1010,.F.);
#1238=ORIENTED_EDGE('',*,*,#1011,.T.);
#1239=ORIENTED_EDGE('',*,*,#1012,.F.);
#1240=ORIENTED_EDGE('',*,*,#1011,.F.);
#1241=ORIENTED_EDGE('',*,*,#1013,.F.);
#1242=ORIENTED_EDGE('',*,*,#1014,.T.);
#1243=ORIENTED_EDGE('',*,*,#1015,.T.);
#1244=ORIENTED_EDGE('',*,*,#1016,.T.);
#1245=ORIENTED_EDGE('',*,*,#1010,.T.);
#1246=ORIENTED_EDGE('',*,*,#1017,.F.);
#1247=ORIENTED_EDGE('',*,*,#1018,.F.);
#1248=ORIENTED_EDGE('',*,*,#1019,.F.);
#1249=ORIENTED_EDGE('',*,*,#1014,.F.);
#1250=ORIENTED_EDGE('',*,*,#1020,.F.);
#1251=ORIENTED_EDGE('',*,*,#1016,.F.);
#1252=ORIENTED_EDGE('',*,*,#1021,.T.);
#1253=ORIENTED_EDGE('',*,*,#1022,.F.);
#1254=ORIENTED_EDGE('',*,*,#1015,.F.);
#1255=ORIENTED_EDGE('',*,*,#1019,.T.);
#1256=ORIENTED_EDGE('',*,*,#1023,.F.);
#1257=ORIENTED_EDGE('',*,*,#1021,.F.);
#1258=ORIENTED_EDGE('',*,*,#1024,.F.);
#1259=ORIENTED_EDGE('',*,*,#1022,.T.);
#1260=ORIENTED_EDGE('',*,*,#1023,.T.);
#1261=ORIENTED_EDGE('',*,*,#1018,.T.);
#1262=ORIENTED_EDGE('',*,*,#1012,.T.);
#1263=ORIENTED_EDGE('',*,*,#1025,.F.);
#1264=ORIENTED_EDGE('',*,*,#1026,.T.);
#1265=ORIENTED_EDGE('',*,*,#1027,.T.);
#1266=ORIENTED_EDGE('',*,*,#1028,.T.);
#1267=ORIENTED_EDGE('',*,*,#1007,.T.);
#1268=ORIENTED_EDGE('',*,*,#1029,.F.);
#1269=ORIENTED_EDGE('',*,*,#1030,.F.);
#1270=ORIENTED_EDGE('',*,*,#1031,.F.);
#1271=ORIENTED_EDGE('',*,*,#1026,.F.);
#1272=ORIENTED_EDGE('',*,*,#1032,.F.);
#1273=ORIENTED_EDGE('',*,*,#1028,.F.);
#1274=ORIENTED_EDGE('',*,*,#1033,.T.);
#1275=ORIENTED_EDGE('',*,*,#1034,.F.);
#1276=ORIENTED_EDGE('',*,*,#1027,.F.);
#1277=ORIENTED_EDGE('',*,*,#1031,.T.);
#1278=ORIENTED_EDGE('',*,*,#1035,.F.);
#1279=ORIENTED_EDGE('',*,*,#1033,.F.);
#1280=ORIENTED_EDGE('',*,*,#1036,.F.);
#1281=ORIENTED_EDGE('',*,*,#1034,.T.);
#1282=ORIENTED_EDGE('',*,*,#1035,.T.);
#1283=ORIENTED_EDGE('',*,*,#1030,.T.);
#1284=ORIENTED_EDGE('',*,*,#1009,.T.);
#1285=ORIENTED_EDGE('',*,*,#1037,.T.);
#1286=ORIENTED_EDGE('',*,*,#1038,.T.);
#1287=ORIENTED_EDGE('',*,*,#1039,.F.);
#1288=ORIENTED_EDGE('',*,*,#1040,.F.);
#1289=ORIENTED_EDGE('',*,*,#1041,.T.);
#1290=ORIENTED_EDGE('',*,*,#1040,.T.);
#1291=ORIENTED_EDGE('',*,*,#1042,.F.);
#1292=ORIENTED_EDGE('',*,*,#1043,.F.);
#1293=ORIENTED_EDGE('',*,*,#1044,.T.);
#1294=ORIENTED_EDGE('',*,*,#1043,.T.);
#1295=ORIENTED_EDGE('',*,*,#1045,.F.);
#1296=ORIENTED_EDGE('',*,*,#1046,.F.);
#1297=ORIENTED_EDGE('',*,*,#1047,.T.);
#1298=ORIENTED_EDGE('',*,*,#1046,.T.);
#1299=ORIENTED_EDGE('',*,*,#1048,.F.);
#1300=ORIENTED_EDGE('',*,*,#1038,.F.);
#1301=ORIENTED_EDGE('',*,*,#1048,.T.);
#1302=ORIENTED_EDGE('',*,*,#1045,.T.);
#1303=ORIENTED_EDGE('',*,*,#1042,.T.);
#1304=ORIENTED_EDGE('',*,*,#1039,.T.);
#1305=ORIENTED_EDGE('',*,*,#1029,.T.);
#1306=ORIENTED_EDGE('',*,*,#1025,.T.);
#1307=ORIENTED_EDGE('',*,*,#1032,.T.);
#1308=ORIENTED_EDGE('',*,*,#1036,.T.);
#1309=ORIENTED_EDGE('',*,*,#1017,.T.);
#1310=ORIENTED_EDGE('',*,*,#1013,.T.);
#1311=ORIENTED_EDGE('',*,*,#1020,.T.);
#1312=ORIENTED_EDGE('',*,*,#1024,.T.);
#1313=ORIENTED_EDGE('',*,*,#1006,.T.);
#1314=ORIENTED_EDGE('',*,*,#1003,.T.);
#1315=ORIENTED_EDGE('',*,*,#1000,.T.);
#1316=ORIENTED_EDGE('',*,*,#997,.T.);
#1317=ORIENTED_EDGE('',*,*,#1047,.F.);
#1318=ORIENTED_EDGE('',*,*,#1037,.F.);
#1319=ORIENTED_EDGE('',*,*,#1041,.F.);
#1320=ORIENTED_EDGE('',*,*,#1044,.F.);
#1321=ORIENTED_EDGE('',*,*,#995,.T.);
#1322=ORIENTED_EDGE('',*,*,#998,.T.);
#1323=ORIENTED_EDGE('',*,*,#1001,.T.);
#1324=ORIENTED_EDGE('',*,*,#1004,.T.);
#1325=ORIENTED_EDGE('',*,*,#1049,.F.);
#1326=ORIENTED_EDGE('',*,*,#1050,.T.);
#1327=ORIENTED_EDGE('',*,*,#1051,.F.);
#1328=ORIENTED_EDGE('',*,*,#1050,.F.);
#1329=ORIENTED_EDGE('',*,*,#1049,.T.);
#1330=ORIENTED_EDGE('',*,*,#1052,.T.);
#1331=ORIENTED_EDGE('',*,*,#1053,.F.);
#1332=ORIENTED_EDGE('',*,*,#1052,.F.);
#1333=ORIENTED_EDGE('',*,*,#1054,.T.);
#1334=ORIENTED_EDGE('',*,*,#1055,.T.);
#1335=ORIENTED_EDGE('',*,*,#1054,.F.);
#1336=ORIENTED_EDGE('',*,*,#1055,.F.);
#1337=ORIENTED_EDGE('',*,*,#1056,.F.);
#1338=ORIENTED_EDGE('',*,*,#1057,.T.);
#1339=ORIENTED_EDGE('',*,*,#1053,.T.);
#1340=ORIENTED_EDGE('',*,*,#1057,.F.);
#1341=ORIENTED_EDGE('',*,*,#1056,.T.);
#1342=ORIENTED_EDGE('',*,*,#1051,.T.);
#1343=ORIENTED_EDGE('',*,*,#1058,.F.);
#1344=ORIENTED_EDGE('',*,*,#1059,.T.);
#1345=ORIENTED_EDGE('',*,*,#1060,.T.);
#1346=ORIENTED_EDGE('',*,*,#1059,.F.);
#1347=ORIENTED_EDGE('',*,*,#1061,.F.);
#1348=ORIENTED_EDGE('',*,*,#1062,.T.);
#1349=ORIENTED_EDGE('',*,*,#1063,.T.);
#1350=ORIENTED_EDGE('',*,*,#1062,.F.);
#1351=ORIENTED_EDGE('',*,*,#1061,.T.);
#1352=ORIENTED_EDGE('',*,*,#1058,.T.);
#1353=ORIENTED_EDGE('',*,*,#1063,.F.);
#1354=ORIENTED_EDGE('',*,*,#1060,.F.);
#1355=ORIENTED_EDGE('',*,*,#1064,.F.);
#1356=ORIENTED_EDGE('',*,*,#1065,.T.);
#1357=ORIENTED_EDGE('',*,*,#1066,.T.);
#1358=ORIENTED_EDGE('',*,*,#1065,.F.);
#1359=ORIENTED_EDGE('',*,*,#1067,.F.);
#1360=ORIENTED_EDGE('',*,*,#1068,.T.);
#1361=ORIENTED_EDGE('',*,*,#1069,.T.);
#1362=ORIENTED_EDGE('',*,*,#1068,.F.);
#1363=ORIENTED_EDGE('',*,*,#1067,.T.);
#1364=ORIENTED_EDGE('',*,*,#1064,.T.);
#1365=ORIENTED_EDGE('',*,*,#1069,.F.);
#1366=ORIENTED_EDGE('',*,*,#1066,.F.);
#1367=ORIENTED_EDGE('',*,*,#1070,.T.);
#1368=ORIENTED_EDGE('',*,*,#1071,.T.);
#1369=ORIENTED_EDGE('',*,*,#1072,.T.);
#1370=ORIENTED_EDGE('',*,*,#1073,.F.);
#1371=ORIENTED_EDGE('',*,*,#1074,.T.);
#1372=ORIENTED_EDGE('',*,*,#1075,.T.);
#1373=ORIENTED_EDGE('',*,*,#1076,.T.);
#1374=ORIENTED_EDGE('',*,*,#1071,.F.);
#1375=ORIENTED_EDGE('',*,*,#1077,.T.);
#1376=ORIENTED_EDGE('',*,*,#1078,.T.);
#1377=ORIENTED_EDGE('',*,*,#1079,.T.);
#1378=ORIENTED_EDGE('',*,*,#1075,.F.);
#1379=ORIENTED_EDGE('',*,*,#1080,.T.);
#1380=ORIENTED_EDGE('',*,*,#1081,.T.);
#1381=ORIENTED_EDGE('',*,*,#1082,.T.);
#1382=ORIENTED_EDGE('',*,*,#1078,.F.);
#1383=ORIENTED_EDGE('',*,*,#1083,.T.);
#1384=ORIENTED_EDGE('',*,*,#1084,.T.);
#1385=ORIENTED_EDGE('',*,*,#1085,.T.);
#1386=ORIENTED_EDGE('',*,*,#1081,.F.);
#1387=ORIENTED_EDGE('',*,*,#1086,.T.);
#1388=ORIENTED_EDGE('',*,*,#1073,.T.);
#1389=ORIENTED_EDGE('',*,*,#1087,.T.);
#1390=ORIENTED_EDGE('',*,*,#1084,.F.);
#1391=ORIENTED_EDGE('',*,*,#1086,.F.);
#1392=ORIENTED_EDGE('',*,*,#1083,.F.);
#1393=ORIENTED_EDGE('',*,*,#1080,.F.);
#1394=ORIENTED_EDGE('',*,*,#1077,.F.);
#1395=ORIENTED_EDGE('',*,*,#1074,.F.);
#1396=ORIENTED_EDGE('',*,*,#1070,.F.);
#1397=ORIENTED_EDGE('',*,*,#1087,.F.);
#1398=ORIENTED_EDGE('',*,*,#1072,.F.);
#1399=ORIENTED_EDGE('',*,*,#1076,.F.);
#1400=ORIENTED_EDGE('',*,*,#1079,.F.);
#1401=ORIENTED_EDGE('',*,*,#1082,.F.);
#1402=ORIENTED_EDGE('',*,*,#1085,.F.);
#1403=ORIENTED_EDGE('',*,*,#1088,.F.);
#1404=ORIENTED_EDGE('',*,*,#1089,.F.);
#1405=ORIENTED_EDGE('',*,*,#1090,.F.);
#1406=ORIENTED_EDGE('',*,*,#1091,.T.);
#1407=ORIENTED_EDGE('',*,*,#1089,.T.);
#1408=ORIENTED_EDGE('',*,*,#1091,.F.);
#1409=ORIENTED_EDGE('',*,*,#1092,.F.);
#1410=ORIENTED_EDGE('',*,*,#1093,.T.);
#1411=ORIENTED_EDGE('',*,*,#1090,.T.);
#1412=ORIENTED_EDGE('',*,*,#1093,.F.);
#1413=ORIENTED_EDGE('',*,*,#1094,.F.);
#1414=ORIENTED_EDGE('',*,*,#1095,.T.);
#1415=ORIENTED_EDGE('',*,*,#1092,.T.);
#1416=ORIENTED_EDGE('',*,*,#1095,.F.);
#1417=ORIENTED_EDGE('',*,*,#1094,.T.);
#1418=ORIENTED_EDGE('',*,*,#1096,.F.);
#1419=ORIENTED_EDGE('',*,*,#1097,.F.);
#1420=ORIENTED_EDGE('',*,*,#1098,.T.);
#1421=ORIENTED_EDGE('',*,*,#1096,.T.);
#1422=ORIENTED_EDGE('',*,*,#1098,.F.);
#1423=ORIENTED_EDGE('',*,*,#1088,.T.);
#1424=ORIENTED_EDGE('',*,*,#1099,.T.);
#1425=ORIENTED_EDGE('',*,*,#1097,.T.);
#1426=ORIENTED_EDGE('',*,*,#1099,.F.);
#1427=ORIENTED_EDGE('',*,*,#1100,.F.);
#1428=ORIENTED_EDGE('',*,*,#1101,.T.);
#1429=ORIENTED_EDGE('',*,*,#1102,.F.);
#1430=ORIENTED_EDGE('',*,*,#1101,.F.);
#1431=ORIENTED_EDGE('',*,*,#1100,.T.);
#1432=ORIENTED_EDGE('',*,*,#1103,.F.);
#1433=ORIENTED_EDGE('',*,*,#1104,.F.);
#1434=ORIENTED_EDGE('',*,*,#1105,.T.);
#1435=ORIENTED_EDGE('',*,*,#1106,.T.);
#1436=ORIENTED_EDGE('',*,*,#1105,.F.);
#1437=ORIENTED_EDGE('',*,*,#1106,.F.);
#1438=ORIENTED_EDGE('',*,*,#1107,.F.);
#1439=ORIENTED_EDGE('',*,*,#1103,.T.);
#1440=ORIENTED_EDGE('',*,*,#1108,.T.);
#1441=ORIENTED_EDGE('',*,*,#1107,.T.);
#1442=ORIENTED_EDGE('',*,*,#1108,.F.);
#1443=ORIENTED_EDGE('',*,*,#1109,.F.);
#1444=ORIENTED_EDGE('',*,*,#1110,.T.);
#1445=ORIENTED_EDGE('',*,*,#1111,.T.);
#1446=ORIENTED_EDGE('',*,*,#1110,.F.);
#1447=ORIENTED_EDGE('',*,*,#1109,.T.);
#1448=ORIENTED_EDGE('',*,*,#1102,.T.);
#1449=ORIENTED_EDGE('',*,*,#1111,.F.);
#1450=ORIENTED_EDGE('',*,*,#1104,.T.);
#1451=ORIENTED_EDGE('',*,*,#1112,.F.);
#1452=ORIENTED_EDGE('',*,*,#1113,.F.);
#1453=ORIENTED_EDGE('',*,*,#1114,.T.);
#1454=ORIENTED_EDGE('',*,*,#1115,.F.);
#1455=ORIENTED_EDGE('',*,*,#1116,.F.);
#1456=ORIENTED_EDGE('',*,*,#1114,.F.);
#1457=ORIENTED_EDGE('',*,*,#1115,.T.);
#1458=ORIENTED_EDGE('',*,*,#1116,.T.);
#1459=ORIENTED_EDGE('',*,*,#1117,.T.);
#1460=ORIENTED_EDGE('',*,*,#1118,.T.);
#1461=ORIENTED_EDGE('',*,*,#1117,.F.);
#1462=ORIENTED_EDGE('',*,*,#1119,.T.);
#1463=ORIENTED_EDGE('',*,*,#1120,.T.);
#1464=ORIENTED_EDGE('',*,*,#1121,.F.);
#1465=ORIENTED_EDGE('',*,*,#1120,.F.);
#1466=ORIENTED_EDGE('',*,*,#1121,.T.);
#1467=ORIENTED_EDGE('',*,*,#1122,.T.);
#1468=ORIENTED_EDGE('',*,*,#1123,.F.);
#1469=ORIENTED_EDGE('',*,*,#1122,.F.);
#1470=ORIENTED_EDGE('',*,*,#1118,.F.);
#1471=ORIENTED_EDGE('',*,*,#1123,.T.);
#1472=ORIENTED_EDGE('',*,*,#1124,.F.);
#1473=ORIENTED_EDGE('',*,*,#1125,.T.);
#1474=ORIENTED_EDGE('',*,*,#1112,.T.);
#1475=ORIENTED_EDGE('',*,*,#1113,.T.);
#1476=ORIENTED_EDGE('',*,*,#1125,.F.);
#1477=ORIENTED_EDGE('',*,*,#1124,.T.);
#1478=ORIENTED_EDGE('',*,*,#1126,.F.);
#1479=ORIENTED_EDGE('',*,*,#1126,.T.);
#1480=ORIENTED_EDGE('',*,*,#1127,.T.);
#1481=ORIENTED_EDGE('',*,*,#1119,.F.);
#1482=ORIENTED_EDGE('',*,*,#1127,.F.);
#1483=ORIENTED_EDGE('',*,*,#1128,.F.);
#1484=ORIENTED_EDGE('',*,*,#1129,.F.);
#1485=ORIENTED_EDGE('',*,*,#1130,.T.);
#1486=ORIENTED_EDGE('',*,*,#1131,.F.);
#1487=ORIENTED_EDGE('',*,*,#1132,.F.);
#1488=ORIENTED_EDGE('',*,*,#1130,.F.);
#1489=ORIENTED_EDGE('',*,*,#1133,.T.);
#1490=ORIENTED_EDGE('',*,*,#1134,.T.);
#1491=ORIENTED_EDGE('',*,*,#1131,.T.);
#1492=ORIENTED_EDGE('',*,*,#1132,.T.);
#1493=ORIENTED_EDGE('',*,*,#1134,.F.);
#1494=ORIENTED_EDGE('',*,*,#1135,.F.);
#1495=ORIENTED_EDGE('',*,*,#1136,.T.);
#1496=ORIENTED_EDGE('',*,*,#1137,.F.);
#1497=ORIENTED_EDGE('',*,*,#1138,.T.);
#1498=ORIENTED_EDGE('',*,*,#1135,.T.);
#1499=ORIENTED_EDGE('',*,*,#1138,.F.);
#1500=ORIENTED_EDGE('',*,*,#1139,.F.);
#1501=ORIENTED_EDGE('',*,*,#1140,.T.);
#1502=ORIENTED_EDGE('',*,*,#1137,.T.);
#1503=ORIENTED_EDGE('',*,*,#1140,.F.);
#1504=ORIENTED_EDGE('',*,*,#1141,.F.);
#1505=ORIENTED_EDGE('',*,*,#1142,.T.);
#1506=ORIENTED_EDGE('',*,*,#1139,.T.);
#1507=ORIENTED_EDGE('',*,*,#1142,.F.);
#1508=ORIENTED_EDGE('',*,*,#1141,.T.);
#1509=ORIENTED_EDGE('',*,*,#1133,.F.);
#1510=ORIENTED_EDGE('',*,*,#1128,.T.);
#1511=ORIENTED_EDGE('',*,*,#1129,.T.);
#1512=ORIENTED_EDGE('',*,*,#1143,.T.);
#1513=ORIENTED_EDGE('',*,*,#1136,.F.);
#1514=ORIENTED_EDGE('',*,*,#1143,.F.);
#1515=ORIENTED_EDGE('',*,*,#1144,.T.);
#1516=ORIENTED_EDGE('',*,*,#1144,.F.);
#1517=ORIENTED_EDGE('',*,*,#1145,.T.);
#1518=ORIENTED_EDGE('',*,*,#1145,.F.);
#1519=ORIENTED_EDGE('',*,*,#1146,.T.);
#1520=ORIENTED_EDGE('',*,*,#1146,.F.);
#1521=ORIENTED_EDGE('',*,*,#1147,.T.);
#1522=ORIENTED_EDGE('',*,*,#1147,.F.);
#1523=ORIENTED_EDGE('',*,*,#1148,.T.);
#1524=ORIENTED_EDGE('',*,*,#1148,.F.);
#1525=ORIENTED_EDGE('',*,*,#1149,.T.);
#1526=ORIENTED_EDGE('',*,*,#1149,.F.);
#1527=ORIENTED_EDGE('',*,*,#1150,.T.);
#1528=ORIENTED_EDGE('',*,*,#1150,.F.);
#1529=ORIENTED_EDGE('',*,*,#1151,.F.);
#1530=ORIENTED_EDGE('',*,*,#1152,.F.);
#1531=ORIENTED_EDGE('',*,*,#1153,.F.);
#1532=ORIENTED_EDGE('',*,*,#1154,.F.);
#1533=ORIENTED_EDGE('',*,*,#1153,.T.);
#1534=ORIENTED_EDGE('',*,*,#1155,.F.);
#1535=ORIENTED_EDGE('',*,*,#1156,.T.);
#1536=ORIENTED_EDGE('',*,*,#1157,.F.);
#1537=ORIENTED_EDGE('',*,*,#1158,.T.);
#1538=ORIENTED_EDGE('',*,*,#1159,.F.);
#1539=ORIENTED_EDGE('',*,*,#1160,.T.);
#1540=ORIENTED_EDGE('',*,*,#1161,.F.);
#1541=ORIENTED_EDGE('',*,*,#1160,.F.);
#1542=ORIENTED_EDGE('',*,*,#1162,.F.);
#1543=ORIENTED_EDGE('',*,*,#1163,.T.);
#1544=ORIENTED_EDGE('',*,*,#1164,.F.);
#1545=ORIENTED_EDGE('',*,*,#1165,.T.);
#1546=ORIENTED_EDGE('',*,*,#1166,.F.);
#1547=ORIENTED_EDGE('',*,*,#1167,.T.);
#1548=ORIENTED_EDGE('',*,*,#1168,.F.);
#1549=ORIENTED_EDGE('',*,*,#1169,.T.);
#1550=ORIENTED_EDGE('',*,*,#1170,.F.);
#1551=ORIENTED_EDGE('',*,*,#1152,.T.);
#1552=ORIENTED_EDGE('',*,*,#1171,.T.);
#1553=ORIENTED_EDGE('',*,*,#1172,.T.);
#1554=ORIENTED_EDGE('',*,*,#1155,.T.);
#1555=ORIENTED_EDGE('',*,*,#1173,.F.);
#1556=ORIENTED_EDGE('',*,*,#1174,.F.);
#1557=ORIENTED_EDGE('',*,*,#1156,.F.);
#1558=ORIENTED_EDGE('',*,*,#1172,.F.);
#1559=ORIENTED_EDGE('',*,*,#1174,.T.);
#1560=ORIENTED_EDGE('',*,*,#1175,.T.);
#1561=ORIENTED_EDGE('',*,*,#1176,.T.);
#1562=ORIENTED_EDGE('',*,*,#1157,.T.);
#1563=ORIENTED_EDGE('',*,*,#1177,.F.);
#1564=ORIENTED_EDGE('',*,*,#1178,.F.);
#1565=ORIENTED_EDGE('',*,*,#1158,.F.);
#1566=ORIENTED_EDGE('',*,*,#1176,.F.);
#1567=ORIENTED_EDGE('',*,*,#1178,.T.);
#1568=ORIENTED_EDGE('',*,*,#1179,.T.);
#1569=ORIENTED_EDGE('',*,*,#1180,.T.);
#1570=ORIENTED_EDGE('',*,*,#1181,.T.);
#1571=ORIENTED_EDGE('',*,*,#1162,.T.);
#1572=ORIENTED_EDGE('',*,*,#1159,.T.);
#1573=ORIENTED_EDGE('',*,*,#1182,.F.);
#1574=ORIENTED_EDGE('',*,*,#1183,.F.);
#1575=ORIENTED_EDGE('',*,*,#1163,.F.);
#1576=ORIENTED_EDGE('',*,*,#1181,.F.);
#1577=ORIENTED_EDGE('',*,*,#1183,.T.);
#1578=ORIENTED_EDGE('',*,*,#1184,.T.);
#1579=ORIENTED_EDGE('',*,*,#1185,.T.);
#1580=ORIENTED_EDGE('',*,*,#1164,.T.);
#1581=ORIENTED_EDGE('',*,*,#1186,.F.);
#1582=ORIENTED_EDGE('',*,*,#1187,.F.);
#1583=ORIENTED_EDGE('',*,*,#1165,.F.);
#1584=ORIENTED_EDGE('',*,*,#1185,.F.);
#1585=ORIENTED_EDGE('',*,*,#1187,.T.);
#1586=ORIENTED_EDGE('',*,*,#1188,.T.);
#1587=ORIENTED_EDGE('',*,*,#1189,.T.);
#1588=ORIENTED_EDGE('',*,*,#1166,.T.);
#1589=ORIENTED_EDGE('',*,*,#1167,.F.);
#1590=ORIENTED_EDGE('',*,*,#1189,.F.);
#1591=ORIENTED_EDGE('',*,*,#1190,.F.);
#1592=ORIENTED_EDGE('',*,*,#1191,.F.);
#1593=ORIENTED_EDGE('',*,*,#1192,.F.);
#1594=ORIENTED_EDGE('',*,*,#1193,.T.);
#1595=ORIENTED_EDGE('',*,*,#1179,.F.);
#1596=ORIENTED_EDGE('',*,*,#1177,.T.);
#1597=ORIENTED_EDGE('',*,*,#1175,.F.);
#1598=ORIENTED_EDGE('',*,*,#1173,.T.);
#1599=ORIENTED_EDGE('',*,*,#1171,.F.);
#1600=ORIENTED_EDGE('',*,*,#1151,.T.);
#1601=ORIENTED_EDGE('',*,*,#1194,.F.);
#1602=ORIENTED_EDGE('',*,*,#1195,.T.);
#1603=ORIENTED_EDGE('',*,*,#1196,.F.);
#1604=ORIENTED_EDGE('',*,*,#1190,.T.);
#1605=ORIENTED_EDGE('',*,*,#1188,.F.);
#1606=ORIENTED_EDGE('',*,*,#1186,.T.);
#1607=ORIENTED_EDGE('',*,*,#1184,.F.);
#1608=ORIENTED_EDGE('',*,*,#1182,.T.);
#1609=ORIENTED_EDGE('',*,*,#1180,.F.);
#1610=ORIENTED_EDGE('',*,*,#1193,.F.);
#1611=ORIENTED_EDGE('',*,*,#1154,.T.);
#1612=ORIENTED_EDGE('',*,*,#1170,.T.);
#1613=ORIENTED_EDGE('',*,*,#1197,.T.);
#1614=ORIENTED_EDGE('',*,*,#1194,.T.);
#1615=ORIENTED_EDGE('',*,*,#1169,.F.);
#1616=ORIENTED_EDGE('',*,*,#1198,.F.);
#1617=ORIENTED_EDGE('',*,*,#1195,.F.);
#1618=ORIENTED_EDGE('',*,*,#1197,.F.);
#1619=ORIENTED_EDGE('',*,*,#1161,.T.);
#1620=ORIENTED_EDGE('',*,*,#1192,.T.);
#1621=ORIENTED_EDGE('',*,*,#1191,.T.);
#1622=ORIENTED_EDGE('',*,*,#1196,.T.);
#1623=ORIENTED_EDGE('',*,*,#1198,.T.);
#1624=ORIENTED_EDGE('',*,*,#1168,.T.);
#1625=ORIENTED_EDGE('',*,*,#1199,.F.);
#1626=ORIENTED_EDGE('',*,*,#1200,.T.);
#1627=ORIENTED_EDGE('',*,*,#1201,.F.);
#1628=ORIENTED_EDGE('',*,*,#1202,.T.);
#1629=ORIENTED_EDGE('',*,*,#1199,.T.);
#1630=ORIENTED_EDGE('',*,*,#1202,.F.);
#1631=ORIENTED_EDGE('',*,*,#1201,.T.);
#1632=ORIENTED_EDGE('',*,*,#1203,.F.);
#1633=ORIENTED_EDGE('',*,*,#1203,.T.);
#1634=ORIENTED_EDGE('',*,*,#1204,.T.);
#1635=ORIENTED_EDGE('',*,*,#1200,.F.);
#1636=ORIENTED_EDGE('',*,*,#1204,.F.);
#1637=ORIENTED_EDGE('',*,*,#1205,.F.);
#1638=ORIENTED_EDGE('',*,*,#1206,.T.);
#1639=ORIENTED_EDGE('',*,*,#1207,.F.);
#1640=ORIENTED_EDGE('',*,*,#1208,.T.);
#1641=ORIENTED_EDGE('',*,*,#1205,.T.);
#1642=ORIENTED_EDGE('',*,*,#1208,.F.);
#1643=ORIENTED_EDGE('',*,*,#1207,.T.);
#1644=ORIENTED_EDGE('',*,*,#1209,.F.);
#1645=ORIENTED_EDGE('',*,*,#1209,.T.);
#1646=ORIENTED_EDGE('',*,*,#1210,.T.);
#1647=ORIENTED_EDGE('',*,*,#1206,.F.);
#1648=ORIENTED_EDGE('',*,*,#1210,.F.);
#1649=ORIENTED_EDGE('',*,*,#1211,.F.);
#1650=ORIENTED_EDGE('',*,*,#1212,.T.);
#1651=ORIENTED_EDGE('',*,*,#1213,.T.);
#1652=ORIENTED_EDGE('',*,*,#1212,.F.);
#1653=ORIENTED_EDGE('',*,*,#1214,.F.);
#1654=ORIENTED_EDGE('',*,*,#1215,.T.);
#1655=ORIENTED_EDGE('',*,*,#1216,.T.);
#1656=ORIENTED_EDGE('',*,*,#1215,.F.);
#1657=ORIENTED_EDGE('',*,*,#1214,.T.);
#1658=ORIENTED_EDGE('',*,*,#1211,.T.);
#1659=ORIENTED_EDGE('',*,*,#1216,.F.);
#1660=ORIENTED_EDGE('',*,*,#1213,.F.);
#1661=CYLINDRICAL_SURFACE('',#1963,0.275);
#1662=CYLINDRICAL_SURFACE('',#1966,0.275);
#1663=CYLINDRICAL_SURFACE('',#1969,0.275);
#1664=CYLINDRICAL_SURFACE('',#1972,0.275);
#1665=CYLINDRICAL_SURFACE('',#1975,0.6);
#1666=CYLINDRICAL_SURFACE('',#1978,0.6);
#1667=CYLINDRICAL_SURFACE('',#1998,0.165);
#1668=CYLINDRICAL_SURFACE('',#2005,0.9);
#1669=CYLINDRICAL_SURFACE('',#2008,0.6);
#1670=CYLINDRICAL_SURFACE('',#2012,0.605);
#1671=CYLINDRICAL_SURFACE('',#2015,0.8);
#1672=CYLINDRICAL_SURFACE('',#2021,0.225);
#1673=CYLINDRICAL_SURFACE('',#2024,0.8);
#1674=CYLINDRICAL_SURFACE('',#2044,0.35);
#1675=CYLINDRICAL_SURFACE('',#2052,0.1954);
#1676=CYLINDRICAL_SURFACE('',#2061,1.6);
#1677=CYLINDRICAL_SURFACE('',#2066,1.6);
#1678=CYLINDRICAL_SURFACE('',#2071,0.62);
#1679=CYLINDRICAL_SURFACE('',#2072,2.5);
#1680=CYLINDRICAL_SURFACE('',#2085,1.070235);
#1681=CYLINDRICAL_SURFACE('',#2087,0.6);
#1682=CYLINDRICAL_SURFACE('',#2093,1.070235);
#1683=CYLINDRICAL_SURFACE('',#2105,1.129765);
#1684=CYLINDRICAL_SURFACE('',#2112,1.6);
#1685=CYLINDRICAL_SURFACE('',#2117,1.129765);
#1686=CYLINDRICAL_SURFACE('',#2137,1.123812);
#1687=CYLINDRICAL_SURFACE('',#2173,1.076188);
#1688=CYLINDRICAL_SURFACE('',#2187,1.119765);
#1689=CYLINDRICAL_SURFACE('',#2191,1.085235);
#1690=CYLINDRICAL_SURFACE('',#2195,1.119765);
#1691=CYLINDRICAL_SURFACE('',#2199,1.085235);
#1692=CYLINDRICAL_SURFACE('',#2206,1.2);
#1693=CYLINDRICAL_SURFACE('',#2209,1.6);
#1694=ADVANCED_FACE('',(#276),#1661,.F.);
#1695=ADVANCED_FACE('',(#277),#1662,.F.);
#1696=ADVANCED_FACE('',(#278),#1663,.F.);
#1697=ADVANCED_FACE('',(#279),#1664,.F.);
#1698=ADVANCED_FACE('',(#280),#1665,.F.);
#1699=ADVANCED_FACE('',(#281),#1666,.F.);
#1700=ADVANCED_FACE('',(#282,#183),#219,.F.);
#1701=ADVANCED_FACE('',(#283),#220,.T.);
#1702=ADVANCED_FACE('',(#284),#221,.T.);
#1703=ADVANCED_FACE('',(#285),#222,.T.);
#1704=ADVANCED_FACE('',(#286,#184),#223,.T.);
#1705=ADVANCED_FACE('',(#287,#185),#224,.F.);
#1706=ADVANCED_FACE('',(#288),#225,.T.);
#1707=ADVANCED_FACE('',(#289),#226,.T.);
#1708=ADVANCED_FACE('',(#290),#227,.T.);
#1709=ADVANCED_FACE('',(#291,#186),#228,.T.);
#1710=ADVANCED_FACE('',(#292),#229,.T.);
#1711=ADVANCED_FACE('',(#293),#230,.T.);
#1712=ADVANCED_FACE('',(#294),#231,.T.);
#1713=ADVANCED_FACE('',(#295),#232,.T.);
#1714=ADVANCED_FACE('',(#296,#187,#188,#189,#190,#191,#192),#233,.T.);
#1715=ADVANCED_FACE('',(#297,#193,#194,#195,#196),#234,.F.);
#1716=ADVANCED_FACE('',(#298),#1667,.F.);
#1717=ADVANCED_FACE('',(#299),#235,.T.);
#1718=ADVANCED_FACE('',(#300,#197),#236,.T.);
#1719=ADVANCED_FACE('',(#301),#1668,.T.);
#1720=ADVANCED_FACE('',(#302),#237,.F.);
#1721=ADVANCED_FACE('',(#303),#1669,.T.);
#1722=ADVANCED_FACE('',(#304,#198),#238,.T.);
#1723=ADVANCED_FACE('',(#305),#1670,.F.);
#1724=ADVANCED_FACE('',(#306),#1671,.T.);
#1725=ADVANCED_FACE('',(#307,#199),#239,.T.);
#1726=ADVANCED_FACE('',(#308,#200),#240,.F.);
#1727=ADVANCED_FACE('',(#309),#1672,.F.);
#1728=ADVANCED_FACE('',(#310),#1673,.T.);
#1729=ADVANCED_FACE('',(#311,#201),#241,.T.);
#1730=ADVANCED_FACE('',(#312,#202),#242,.F.);
#1731=ADVANCED_FACE('',(#313),#243,.F.);
#1732=ADVANCED_FACE('',(#314),#244,.F.);
#1733=ADVANCED_FACE('',(#315),#245,.F.);
#1734=ADVANCED_FACE('',(#316),#246,.F.);
#1735=ADVANCED_FACE('',(#317),#247,.F.);
#1736=ADVANCED_FACE('',(#318),#248,.F.);
#1737=ADVANCED_FACE('',(#319),#249,.F.);
#1738=ADVANCED_FACE('',(#320),#250,.F.);
#1739=ADVANCED_FACE('',(#321),#251,.F.);
#1740=ADVANCED_FACE('',(#322),#252,.T.);
#1741=ADVANCED_FACE('',(#323),#113,.T.);
#1742=ADVANCED_FACE('',(#324),#1674,.T.);
#1743=ADVANCED_FACE('',(#325),#114,.T.);
#1744=ADVANCED_FACE('',(#326,#203),#253,.T.);
#1745=ADVANCED_FACE('',(#327),#115,.T.);
#1746=ADVANCED_FACE('',(#328),#1675,.T.);
#1747=ADVANCED_FACE('',(#329),#1676,.F.);
#1748=ADVANCED_FACE('',(#330,#204),#254,.T.);
#1749=ADVANCED_FACE('',(#331),#1677,.F.);
#1750=ADVANCED_FACE('',(#332,#205),#255,.F.);
#1751=ADVANCED_FACE('',(#333),#1678,.F.);
#1752=ADVANCED_FACE('',(#334),#1679,.T.);
#1753=ADVANCED_FACE('',(#335,#206),#256,.T.);
#1754=ADVANCED_FACE('',(#336,#207),#257,.F.);
#1755=ADVANCED_FACE('',(#337),#39,.F.);
#1756=ADVANCED_FACE('',(#338),#1680,.T.);
#1757=ADVANCED_FACE('',(#339),#1681,.F.);
#1758=ADVANCED_FACE('',(#340),#116,.F.);
#1759=ADVANCED_FACE('',(#341,#208),#258,.T.);
#1760=ADVANCED_FACE('',(#342),#1682,.T.);
#1761=ADVANCED_FACE('',(#343,#209),#259,.T.);
#1762=ADVANCED_FACE('',(#344),#117,.F.);
#1763=ADVANCED_FACE('',(#345),#40,.F.);
#1764=ADVANCED_FACE('',(#346),#1683,.F.);
#1765=ADVANCED_FACE('',(#347,#210),#260,.T.);
#1766=ADVANCED_FACE('',(#348),#118,.T.);
#1767=ADVANCED_FACE('',(#349),#1684,.T.);
#1768=ADVANCED_FACE('',(#350),#119,.T.);
#1769=ADVANCED_FACE('',(#351,#211),#261,.T.);
#1770=ADVANCED_FACE('',(#352),#1685,.F.);
#1771=ADVANCED_FACE('',(#353),#25,.T.);
#1772=ADVANCED_FACE('',(#354),#26,.T.);
#1773=ADVANCED_FACE('',(#355),#27,.T.);
#1774=ADVANCED_FACE('',(#356),#28,.T.);
#1775=ADVANCED_FACE('',(#357),#29,.T.);
#1776=ADVANCED_FACE('',(#358),#30,.T.);
#1777=ADVANCED_FACE('',(#359),#31,.T.);
#1778=ADVANCED_FACE('',(#360),#32,.F.);
#1779=ADVANCED_FACE('',(#361),#1686,.T.);
#1780=ADVANCED_FACE('',(#362),#262,.T.);
#1781=ADVANCED_FACE('',(#363),#33,.F.);
#1782=ADVANCED_FACE('',(#364),#263,.T.);
#1783=ADVANCED_FACE('',(#365),#34,.F.);
#1784=ADVANCED_FACE('',(#366),#264,.T.);
#1785=ADVANCED_FACE('',(#367),#35,.F.);
#1786=ADVANCED_FACE('',(#368),#265,.T.);
#1787=ADVANCED_FACE('',(#369),#36,.F.);
#1788=ADVANCED_FACE('',(#370),#266,.T.);
#1789=ADVANCED_FACE('',(#371),#37,.F.);
#1790=ADVANCED_FACE('',(#372),#1687,.F.);
#1791=ADVANCED_FACE('',(#373),#267,.T.);
#1792=ADVANCED_FACE('',(#374),#38,.F.);
#1793=ADVANCED_FACE('',(#375,#212),#268,.T.);
#1794=ADVANCED_FACE('',(#376),#269,.T.);
#1795=ADVANCED_FACE('',(#377,#213),#270,.T.);
#1796=ADVANCED_FACE('',(#378),#1688,.T.);
#1797=ADVANCED_FACE('',(#379,#214),#271,.T.);
#1798=ADVANCED_FACE('',(#380),#1689,.F.);
#1799=ADVANCED_FACE('',(#381,#215),#272,.T.);
#1800=ADVANCED_FACE('',(#382),#1690,.T.);
#1801=ADVANCED_FACE('',(#383,#216),#273,.T.);
#1802=ADVANCED_FACE('',(#384),#1691,.F.);
#1803=ADVANCED_FACE('',(#385),#1692,.F.);
#1804=ADVANCED_FACE('',(#386),#1693,.T.);
#1805=ADVANCED_FACE('',(#387,#217),#274,.T.);
#1806=ADVANCED_FACE('',(#388,#218),#275,.F.);
#1807=CLOSED_SHELL('',(#1694,#1695,#1696,#1697,#1698,#1699,#1700,#1701,
#1702,#1703,#1704,#1705,#1706,#1707,#1708,#1709,#1710,#1711,#1712,#1713,
#1714,#1715));
#1808=CLOSED_SHELL('',(#1716,#1717,#1718,#1719,#1720,#1721,#1722));
#1809=CLOSED_SHELL('',(#1723,#1724,#1725,#1726));
#1810=CLOSED_SHELL('',(#1727,#1728,#1729,#1730));
#1811=CLOSED_SHELL('',(#1731,#1732,#1733,#1734,#1735,#1736,#1737,#1738));
#1812=CLOSED_SHELL('',(#1739,#1740,#1741,#1742,#1743,#1744,#1745,#1746));
#1813=CLOSED_SHELL('',(#1747,#1748,#1749,#1750,#1751,#1752,#1753,#1754));
#1814=CLOSED_SHELL('',(#1755,#1756,#1757,#1758,#1759,#1760,#1761,#1762));
#1815=CLOSED_SHELL('',(#1763,#1764,#1765,#1766,#1767,#1768,#1769,#1770));
#1816=CLOSED_SHELL('',(#1771));
#1817=CLOSED_SHELL('',(#1772));
#1818=CLOSED_SHELL('',(#1773));
#1819=CLOSED_SHELL('',(#1774));
#1820=CLOSED_SHELL('',(#1775));
#1821=CLOSED_SHELL('',(#1776));
#1822=CLOSED_SHELL('',(#1777));
#1823=CLOSED_SHELL('',(#1778,#1779,#1780,#1781,#1782,#1783,#1784,#1785,
#1786,#1787,#1788,#1789,#1790,#1791,#1792,#1793,#1794));
#1824=CLOSED_SHELL('',(#1795,#1796,#1797,#1798));
#1825=CLOSED_SHELL('',(#1799,#1800,#1801,#1802));
#1826=CLOSED_SHELL('',(#1803,#1804,#1805,#1806));
#1827=DERIVED_UNIT_ELEMENT(#1851,1.);
#1828=DERIVED_UNIT_ELEMENT(#3690,-3.);
#1829=DERIVED_UNIT_ELEMENT(#1851,1.);
#1830=DERIVED_UNIT_ELEMENT(#3690,-3.);
#1831=DERIVED_UNIT_ELEMENT(#1851,1.);
#1832=DERIVED_UNIT_ELEMENT(#3690,-3.);
#1833=DERIVED_UNIT_ELEMENT(#1851,1.);
#1834=DERIVED_UNIT_ELEMENT(#3690,-3.);
#1835=DERIVED_UNIT_ELEMENT(#1851,1.);
#1836=DERIVED_UNIT_ELEMENT(#3690,-3.);
#1837=DERIVED_UNIT_ELEMENT(#1851,1.);
#1838=DERIVED_UNIT_ELEMENT(#3690,-3.);
#1839=DERIVED_UNIT_ELEMENT(#1851,1.);
#1840=DERIVED_UNIT_ELEMENT(#3690,-3.);
#1841=DERIVED_UNIT_ELEMENT(#1851,1.);
#1842=DERIVED_UNIT_ELEMENT(#3690,-3.);
#1843=DERIVED_UNIT_ELEMENT(#1851,1.);
#1844=DERIVED_UNIT_ELEMENT(#3690,-3.);
#1845=DERIVED_UNIT_ELEMENT(#1851,1.);
#1846=DERIVED_UNIT_ELEMENT(#3690,-3.);
#1847=DERIVED_UNIT_ELEMENT(#1851,1.);
#1848=DERIVED_UNIT_ELEMENT(#3690,-3.);
#1849=DERIVED_UNIT_ELEMENT(#1851,1.);
#1850=DERIVED_UNIT_ELEMENT(#3690,-3.);
#1851=(
MASS_UNIT()
NAMED_UNIT(*)
SI_UNIT(.KILO.,.GRAM.)
);
#1852=DERIVED_UNIT((#1827,#1828));
#1853=DERIVED_UNIT((#1829,#1830));
#1854=DERIVED_UNIT((#1831,#1832));
#1855=DERIVED_UNIT((#1833,#1834));
#1856=DERIVED_UNIT((#1835,#1836));
#1857=DERIVED_UNIT((#1837,#1838));
#1858=DERIVED_UNIT((#1839,#1840));
#1859=DERIVED_UNIT((#1841,#1842));
#1860=DERIVED_UNIT((#1843,#1844));
#1861=DERIVED_UNIT((#1845,#1846));
#1862=DERIVED_UNIT((#1847,#1848));
#1863=DERIVED_UNIT((#1849,#1850));
#1864=MEASURE_REPRESENTATION_ITEM('density measure',
POSITIVE_RATIO_MEASURE(7850.),#1852);
#1865=MEASURE_REPRESENTATION_ITEM('density measure',
POSITIVE_RATIO_MEASURE(7850.),#1853);
#1866=MEASURE_REPRESENTATION_ITEM('density measure',
POSITIVE_RATIO_MEASURE(7850.),#1854);
#1867=MEASURE_REPRESENTATION_ITEM('density measure',
POSITIVE_RATIO_MEASURE(7850.),#1855);
#1868=MEASURE_REPRESENTATION_ITEM('density measure',
POSITIVE_RATIO_MEASURE(7850.),#1856);
#1869=MEASURE_REPRESENTATION_ITEM('density measure',
POSITIVE_RATIO_MEASURE(7850.),#1857);
#1870=MEASURE_REPRESENTATION_ITEM('density measure',
POSITIVE_RATIO_MEASURE(7850.),#1858);
#1871=MEASURE_REPRESENTATION_ITEM('density measure',
POSITIVE_RATIO_MEASURE(7850.),#1859);
#1872=MEASURE_REPRESENTATION_ITEM('density measure',
POSITIVE_RATIO_MEASURE(7850.),#1860);
#1873=MEASURE_REPRESENTATION_ITEM('density measure',
POSITIVE_RATIO_MEASURE(7850.),#1861);
#1874=MEASURE_REPRESENTATION_ITEM('density measure',
POSITIVE_RATIO_MEASURE(7850.),#1862);
#1875=MEASURE_REPRESENTATION_ITEM('density measure',
POSITIVE_RATIO_MEASURE(7850.),#1863);
#1876=PROPERTY_DEFINITION_REPRESENTATION(#1936,#1900);
#1877=PROPERTY_DEFINITION_REPRESENTATION(#1937,#1901);
#1878=PROPERTY_DEFINITION_REPRESENTATION(#1938,#1902);
#1879=PROPERTY_DEFINITION_REPRESENTATION(#1939,#1903);
#1880=PROPERTY_DEFINITION_REPRESENTATION(#1940,#1904);
#1881=PROPERTY_DEFINITION_REPRESENTATION(#1941,#1905);
#1882=PROPERTY_DEFINITION_REPRESENTATION(#1942,#1906);
#1883=PROPERTY_DEFINITION_REPRESENTATION(#1943,#1907);
#1884=PROPERTY_DEFINITION_REPRESENTATION(#1944,#1908);
#1885=PROPERTY_DEFINITION_REPRESENTATION(#1945,#1909);
#1886=PROPERTY_DEFINITION_REPRESENTATION(#1946,#1910);
#1887=PROPERTY_DEFINITION_REPRESENTATION(#1947,#1911);
#1888=PROPERTY_DEFINITION_REPRESENTATION(#1948,#1912);
#1889=PROPERTY_DEFINITION_REPRESENTATION(#1949,#1913);
#1890=PROPERTY_DEFINITION_REPRESENTATION(#1950,#1914);
#1891=PROPERTY_DEFINITION_REPRESENTATION(#1951,#1915);
#1892=PROPERTY_DEFINITION_REPRESENTATION(#1952,#1916);
#1893=PROPERTY_DEFINITION_REPRESENTATION(#1953,#1917);
#1894=PROPERTY_DEFINITION_REPRESENTATION(#1954,#1918);
#1895=PROPERTY_DEFINITION_REPRESENTATION(#1955,#1919);
#1896=PROPERTY_DEFINITION_REPRESENTATION(#1956,#1920);
#1897=PROPERTY_DEFINITION_REPRESENTATION(#1957,#1921);
#1898=PROPERTY_DEFINITION_REPRESENTATION(#1958,#1922);
#1899=PROPERTY_DEFINITION_REPRESENTATION(#1959,#1923);
#1900=REPRESENTATION('material name',(#1924),#3674);
#1901=REPRESENTATION('density',(#1864),#3674);
#1902=REPRESENTATION('material name',(#1925),#3675);
#1903=REPRESENTATION('density',(#1865),#3675);
#1904=REPRESENTATION('material name',(#1926),#3676);
#1905=REPRESENTATION('density',(#1866),#3676);
#1906=REPRESENTATION('material name',(#1927),#3677);
#1907=REPRESENTATION('density',(#1867),#3677);
#1908=REPRESENTATION('material name',(#1928),#3678);
#1909=REPRESENTATION('density',(#1868),#3678);
#1910=REPRESENTATION('material name',(#1929),#3680);
#1911=REPRESENTATION('density',(#1869),#3680);
#1912=REPRESENTATION('material name',(#1930),#3682);
#1913=REPRESENTATION('density',(#1870),#3682);
#1914=REPRESENTATION('material name',(#1931),#3683);
#1915=REPRESENTATION('density',(#1871),#3683);
#1916=REPRESENTATION('material name',(#1932),#3684);
#1917=REPRESENTATION('density',(#1872),#3684);
#1918=REPRESENTATION('material name',(#1933),#3685);
#1919=REPRESENTATION('density',(#1873),#3685);
#1920=REPRESENTATION('material name',(#1934),#3686);
#1921=REPRESENTATION('density',(#1874),#3686);
#1922=REPRESENTATION('material name',(#1935),#3687);
#1923=REPRESENTATION('density',(#1875),#3687);
#1924=DESCRIPTIVE_REPRESENTATION_ITEM('Steel','Steel');
#1925=DESCRIPTIVE_REPRESENTATION_ITEM('Steel','Steel');
#1926=DESCRIPTIVE_REPRESENTATION_ITEM('Steel','Steel');
#1927=DESCRIPTIVE_REPRESENTATION_ITEM('Steel','Steel');
#1928=DESCRIPTIVE_REPRESENTATION_ITEM('Steel','Steel');
#1929=DESCRIPTIVE_REPRESENTATION_ITEM('Steel','Steel');
#1930=DESCRIPTIVE_REPRESENTATION_ITEM('Steel','Steel');
#1931=DESCRIPTIVE_REPRESENTATION_ITEM('Steel','Steel');
#1932=DESCRIPTIVE_REPRESENTATION_ITEM('Steel','Steel');
#1933=DESCRIPTIVE_REPRESENTATION_ITEM('Steel','Steel');
#1934=DESCRIPTIVE_REPRESENTATION_ITEM('Steel','Steel');
#1935=DESCRIPTIVE_REPRESENTATION_ITEM('Steel','Steel');
#1936=PROPERTY_DEFINITION('material property','material name',#3762);
#1937=PROPERTY_DEFINITION('material property','density of part',#3762);
#1938=PROPERTY_DEFINITION('material property','material name',#3763);
#1939=PROPERTY_DEFINITION('material property','density of part',#3763);
#1940=PROPERTY_DEFINITION('material property','material name',#3764);
#1941=PROPERTY_DEFINITION('material property','density of part',#3764);
#1942=PROPERTY_DEFINITION('material property','material name',#3765);
#1943=PROPERTY_DEFINITION('material property','density of part',#3765);
#1944=PROPERTY_DEFINITION('material property','material name',#3766);
#1945=PROPERTY_DEFINITION('material property','density of part',#3766);
#1946=PROPERTY_DEFINITION('material property','material name',#3768);
#1947=PROPERTY_DEFINITION('material property','density of part',#3768);
#1948=PROPERTY_DEFINITION('material property','material name',#3770);
#1949=PROPERTY_DEFINITION('material property','density of part',#3770);
#1950=PROPERTY_DEFINITION('material property','material name',#3771);
#1951=PROPERTY_DEFINITION('material property','density of part',#3771);
#1952=PROPERTY_DEFINITION('material property','material name',#3772);
#1953=PROPERTY_DEFINITION('material property','density of part',#3772);
#1954=PROPERTY_DEFINITION('material property','material name',#3773);
#1955=PROPERTY_DEFINITION('material property','density of part',#3773);
#1956=PROPERTY_DEFINITION('material property','material name',#3774);
#1957=PROPERTY_DEFINITION('material property','density of part',#3774);
#1958=PROPERTY_DEFINITION('material property','material name',#3775);
#1959=PROPERTY_DEFINITION('material property','density of part',#3775);
#1960=AXIS2_PLACEMENT_3D('',#2837,#2221,#2222);
#1961=AXIS2_PLACEMENT_3D('',#2838,#2223,#2224);
#1962=AXIS2_PLACEMENT_3D('',#2839,#2225,#2226);
#1963=AXIS2_PLACEMENT_3D('',#2840,#2227,#2228);
#1964=AXIS2_PLACEMENT_3D('',#2842,#2229,#2230);
#1965=AXIS2_PLACEMENT_3D('',#2845,#2232,#2233);
#1966=AXIS2_PLACEMENT_3D('',#2846,#2234,#2235);
#1967=AXIS2_PLACEMENT_3D('',#2848,#2236,#2237);
#1968=AXIS2_PLACEMENT_3D('',#2851,#2239,#2240);
#1969=AXIS2_PLACEMENT_3D('',#2852,#2241,#2242);
#1970=AXIS2_PLACEMENT_3D('',#2854,#2243,#2244);
#1971=AXIS2_PLACEMENT_3D('',#2857,#2246,#2247);
#1972=AXIS2_PLACEMENT_3D('',#2858,#2248,#2249);
#1973=AXIS2_PLACEMENT_3D('',#2860,#2250,#2251);
#1974=AXIS2_PLACEMENT_3D('',#2863,#2253,#2254);
#1975=AXIS2_PLACEMENT_3D('',#2864,#2255,#2256);
#1976=AXIS2_PLACEMENT_3D('',#2866,#2257,#2258);
#1977=AXIS2_PLACEMENT_3D('',#2869,#2260,#2261);
#1978=AXIS2_PLACEMENT_3D('',#2870,#2262,#2263);
#1979=AXIS2_PLACEMENT_3D('',#2872,#2264,#2265);
#1980=AXIS2_PLACEMENT_3D('',#2875,#2267,#2268);
#1981=AXIS2_PLACEMENT_3D('',#2876,#2269,#2270);
#1982=AXIS2_PLACEMENT_3D('',#2885,#2275,#2276);
#1983=AXIS2_PLACEMENT_3D('',#2891,#2280,#2281);
#1984=AXIS2_PLACEMENT_3D('',#2897,#2285,#2286);
#1985=AXIS2_PLACEMENT_3D('',#2899,#2288,#2289);
#1986=AXIS2_PLACEMENT_3D('',#2901,#2291,#2292);
#1987=AXIS2_PLACEMENT_3D('',#2910,#2297,#2298);
#1988=AXIS2_PLACEMENT_3D('',#2916,#2302,#2303);
#1989=AXIS2_PLACEMENT_3D('',#2922,#2307,#2308);
#1990=AXIS2_PLACEMENT_3D('',#2924,#2310,#2311);
#1991=AXIS2_PLACEMENT_3D('',#2926,#2313,#2314);
#1992=AXIS2_PLACEMENT_3D('',#2935,#2319,#2320);
#1993=AXIS2_PLACEMENT_3D('',#2941,#2324,#2325);
#1994=AXIS2_PLACEMENT_3D('',#2947,#2329,#2330);
#1995=AXIS2_PLACEMENT_3D('',#2950,#2333,#2334);
#1996=AXIS2_PLACEMENT_3D('',#2951,#2335,#2336);
#1997=AXIS2_PLACEMENT_3D('',#2952,#2337,#2338);
#1998=AXIS2_PLACEMENT_3D('',#2953,#2339,#2340);
#1999=AXIS2_PLACEMENT_3D('',#2955,#2341,#2342);
#2000=AXIS2_PLACEMENT_3D('',#2958,#2344,#2345);
#2001=AXIS2_PLACEMENT_3D('',#2959,#2346,#2347);
#2002=AXIS2_PLACEMENT_3D('',#2960,#2348,#2349);
#2003=AXIS2_PLACEMENT_3D('',#2962,#2350,#2351);
#2004=AXIS2_PLACEMENT_3D('',#2964,#2352,#2353);
#2005=AXIS2_PLACEMENT_3D('',#2965,#2354,#2355);
#2006=AXIS2_PLACEMENT_3D('',#2968,#2357,#2358);
#2007=AXIS2_PLACEMENT_3D('',#2969,#2359,#2360);
#2008=AXIS2_PLACEMENT_3D('',#2970,#2361,#2362);
#2009=AXIS2_PLACEMENT_3D('',#2972,#2363,#2364);
#2010=AXIS2_PLACEMENT_3D('',#2974,#2366,#2367);
#2011=AXIS2_PLACEMENT_3D('',#2975,#2368,#2369);
#2012=AXIS2_PLACEMENT_3D('',#2976,#2370,#2371);
#2013=AXIS2_PLACEMENT_3D('',#2978,#2372,#2373);
#2014=AXIS2_PLACEMENT_3D('',#2981,#2375,#2376);
#2015=AXIS2_PLACEMENT_3D('',#2982,#2377,#2378);
#2016=AXIS2_PLACEMENT_3D('',#2984,#2379,#2380);
#2017=AXIS2_PLACEMENT_3D('',#2987,#2382,#2383);
#2018=AXIS2_PLACEMENT_3D('',#2988,#2384,#2385);
#2019=AXIS2_PLACEMENT_3D('',#2989,#2386,#2387);
#2020=AXIS2_PLACEMENT_3D('',#2990,#2388,#2389);
#2021=AXIS2_PLACEMENT_3D('',#2991,#2390,#2391);
#2022=AXIS2_PLACEMENT_3D('',#2993,#2392,#2393);
#2023=AXIS2_PLACEMENT_3D('',#2996,#2395,#2396);
#2024=AXIS2_PLACEMENT_3D('',#2997,#2397,#2398);
#2025=AXIS2_PLACEMENT_3D('',#2999,#2399,#2400);
#2026=AXIS2_PLACEMENT_3D('',#3002,#2402,#2403);
#2027=AXIS2_PLACEMENT_3D('',#3003,#2404,#2405);
#2028=AXIS2_PLACEMENT_3D('',#3004,#2406,#2407);
#2029=AXIS2_PLACEMENT_3D('',#3005,#2408,#2409);
#2030=AXIS2_PLACEMENT_3D('',#3006,#2410,#2411);
#2031=AXIS2_PLACEMENT_3D('',#3015,#2416,#2417);
#2032=AXIS2_PLACEMENT_3D('',#3021,#2421,#2422);
#2033=AXIS2_PLACEMENT_3D('',#3027,#2426,#2427);
#2034=AXIS2_PLACEMENT_3D('',#3033,#2431,#2432);
#2035=AXIS2_PLACEMENT_3D('',#3039,#2436,#2437);
#2036=AXIS2_PLACEMENT_3D('',#3042,#2440,#2441);
#2037=AXIS2_PLACEMENT_3D('',#3043,#2442,#2443);
#2038=AXIS2_PLACEMENT_3D('',#3044,#2444,#2445);
#2039=AXIS2_PLACEMENT_3D('',#3046,#2446,#2447);
#2040=AXIS2_PLACEMENT_3D('',#3047,#2448,#2449);
#2041=AXIS2_PLACEMENT_3D('',#3049,#2450,#2451);
#2042=AXIS2_PLACEMENT_3D('',#3050,#2452,#2453);
#2043=AXIS2_PLACEMENT_3D('',#3052,#2454,#2455);
#2044=AXIS2_PLACEMENT_3D('',#3054,#2457,#2458);
#2045=AXIS2_PLACEMENT_3D('',#3056,#2459,#2460);
#2046=AXIS2_PLACEMENT_3D('',#3058,#2462,#2463);
#2047=AXIS2_PLACEMENT_3D('',#3060,#2464,#2465);
#2048=AXIS2_PLACEMENT_3D('',#3062,#2467,#2468);
#2049=AXIS2_PLACEMENT_3D('',#3064,#2469,#2470);
#2050=AXIS2_PLACEMENT_3D('',#3065,#2471,#2472);
#2051=AXIS2_PLACEMENT_3D('',#3067,#2473,#2474);
#2052=AXIS2_PLACEMENT_3D('',#3069,#2476,#2477);
#2053=AXIS2_PLACEMENT_3D('',#3071,#2479,#2480);
#2054=AXIS2_PLACEMENT_3D('',#3072,#2481,#2482);
#2055=AXIS2_PLACEMENT_3D('',#3073,#2483,#2484);
#2056=AXIS2_PLACEMENT_3D('',#3074,#2485,#2486);
#2057=AXIS2_PLACEMENT_3D('',#3075,#2487,#2488);
#2058=AXIS2_PLACEMENT_3D('',#3076,#2489,#2490);
#2059=AXIS2_PLACEMENT_3D('',#3077,#2491,#2492);
#2060=AXIS2_PLACEMENT_3D('',#3078,#2493,#2494);
#2061=AXIS2_PLACEMENT_3D('',#3079,#2495,#2496);
#2062=AXIS2_PLACEMENT_3D('',#3081,#2497,#2498);
#2063=AXIS2_PLACEMENT_3D('',#3084,#2500,#2501);
#2064=AXIS2_PLACEMENT_3D('',#3085,#2502,#2503);
#2065=AXIS2_PLACEMENT_3D('',#3087,#2504,#2505);
#2066=AXIS2_PLACEMENT_3D('',#3088,#2506,#2507);
#2067=AXIS2_PLACEMENT_3D('',#3090,#2508,#2509);
#2068=AXIS2_PLACEMENT_3D('',#3093,#2511,#2512);
#2069=AXIS2_PLACEMENT_3D('',#3094,#2513,#2514);
#2070=AXIS2_PLACEMENT_3D('',#3096,#2515,#2516);
#2071=AXIS2_PLACEMENT_3D('',#3097,#2517,#2518);
#2072=AXIS2_PLACEMENT_3D('',#3099,#2520,#2521);
#2073=AXIS2_PLACEMENT_3D('',#3101,#2522,#2523);
#2074=AXIS2_PLACEMENT_3D('',#3104,#2525,#2526);
#2075=AXIS2_PLACEMENT_3D('',#3105,#2527,#2528);
#2076=AXIS2_PLACEMENT_3D('',#3106,#2529,#2530);
#2077=AXIS2_PLACEMENT_3D('',#3107,#2531,#2532);
#2078=AXIS2_PLACEMENT_3D('',#3108,#2533,#2534);
#2079=AXIS2_PLACEMENT_3D('',#3109,#2535,#2536);
#2080=AXIS2_PLACEMENT_3D('',#3112,#2537,#2538);
#2081=AXIS2_PLACEMENT_3D('',#3113,#2539,#2540);
#2082=AXIS2_PLACEMENT_3D('',#3115,#2541,#2542);
#2083=AXIS2_PLACEMENT_3D('',#3117,#2543,#2544);
#2084=AXIS2_PLACEMENT_3D('',#3118,#2545,#2546);
#2085=AXIS2_PLACEMENT_3D('',#3119,#2547,#2548);
#2086=AXIS2_PLACEMENT_3D('',#3122,#2550,#2551);
#2087=AXIS2_PLACEMENT_3D('',#3123,#2552,#2553);
#2088=AXIS2_PLACEMENT_3D('',#3125,#2554,#2555);
#2089=AXIS2_PLACEMENT_3D('',#3128,#2557,#2558);
#2090=AXIS2_PLACEMENT_3D('',#3129,#2559,#2560);
#2091=AXIS2_PLACEMENT_3D('',#3132,#2562,#2563);
#2092=AXIS2_PLACEMENT_3D('',#3133,#2564,#2565);
#2093=AXIS2_PLACEMENT_3D('',#3134,#2566,#2567);
#2094=AXIS2_PLACEMENT_3D('',#3136,#2568,#2569);
#2095=AXIS2_PLACEMENT_3D('',#3138,#2571,#2572);
#2096=AXIS2_PLACEMENT_3D('',#3140,#2573,#2574);
#2097=AXIS2_PLACEMENT_3D('',#3141,#2575,#2576);
#2098=AXIS2_PLACEMENT_3D('',#3143,#2578,#2579);
#2099=AXIS2_PLACEMENT_3D('',#3144,#2580,#2581);
#2100=AXIS2_PLACEMENT_3D('',#3147,#2582,#2583);
#2101=AXIS2_PLACEMENT_3D('',#3148,#2584,#2585);
#2102=AXIS2_PLACEMENT_3D('',#3150,#2586,#2587);
#2103=AXIS2_PLACEMENT_3D('',#3152,#2588,#2589);
#2104=AXIS2_PLACEMENT_3D('',#3153,#2590,#2591);
#2105=AXIS2_PLACEMENT_3D('',#3154,#2592,#2593);
#2106=AXIS2_PLACEMENT_3D('',#3156,#2594,#2595);
#2107=AXIS2_PLACEMENT_3D('',#3158,#2597,#2598);
#2108=AXIS2_PLACEMENT_3D('',#3160,#2599,#2600);
#2109=AXIS2_PLACEMENT_3D('',#3162,#2601,#2602);
#2110=AXIS2_PLACEMENT_3D('',#3163,#2603,#2604);
#2111=AXIS2_PLACEMENT_3D('',#3165,#2605,#2606);
#2112=AXIS2_PLACEMENT_3D('',#3167,#2608,#2609);
#2113=AXIS2_PLACEMENT_3D('',#3169,#2610,#2611);
#2114=AXIS2_PLACEMENT_3D('',#3171,#2613,#2614);
#2115=AXIS2_PLACEMENT_3D('',#3173,#2615,#2616);
#2116=AXIS2_PLACEMENT_3D('',#3175,#2618,#2619);
#2117=AXIS2_PLACEMENT_3D('',#3176,#2620,#2621);
#2118=AXIS2_PLACEMENT_3D('',#3178,#2623,#2624);
#2119=AXIS2_PLACEMENT_3D('',#3179,#2625,#2626);
#2120=AXIS2_PLACEMENT_3D('',#3182,#2627,#2628);
#2121=AXIS2_PLACEMENT_3D('',#3183,#2629,#2630);
#2122=AXIS2_PLACEMENT_3D('',#3186,#2631,#2632);
#2123=AXIS2_PLACEMENT_3D('',#3187,#2633,#2634);
#2124=AXIS2_PLACEMENT_3D('',#3190,#2635,#2636);
#2125=AXIS2_PLACEMENT_3D('',#3191,#2637,#2638);
#2126=AXIS2_PLACEMENT_3D('',#3194,#2639,#2640);
#2127=AXIS2_PLACEMENT_3D('',#3195,#2641,#2642);
#2128=AXIS2_PLACEMENT_3D('',#3198,#2643,#2644);
#2129=AXIS2_PLACEMENT_3D('',#3199,#2645,#2646);
#2130=AXIS2_PLACEMENT_3D('',#3202,#2647,#2648);
#2131=AXIS2_PLACEMENT_3D('',#3203,#2649,#2650);
#2132=AXIS2_PLACEMENT_3D('',#3206,#2651,#2652);
#2133=AXIS2_PLACEMENT_3D('',#3207,#2653,#2654);
#2134=AXIS2_PLACEMENT_3D('',#3208,#2655,#2656);
#2135=AXIS2_PLACEMENT_3D('',#3234,#2657,#2658);
#2136=AXIS2_PLACEMENT_3D('',#3258,#2659,#2660);
#2137=AXIS2_PLACEMENT_3D('',#3259,#2661,#2662);
#2138=AXIS2_PLACEMENT_3D('',#3261,#2663,#2664);
#2139=AXIS2_PLACEMENT_3D('',#3286,#2665,#2666);
#2140=AXIS2_PLACEMENT_3D('',#3311,#2667,#2668);
#2141=AXIS2_PLACEMENT_3D('',#3314,#2670,#2671);
#2142=AXIS2_PLACEMENT_3D('',#3316,#2672,#2673);
#2143=AXIS2_PLACEMENT_3D('',#3341,#2674,#2675);
#2144=AXIS2_PLACEMENT_3D('',#3366,#2676,#2677);
#2145=AXIS2_PLACEMENT_3D('',#3391,#2678,#2679);
#2146=AXIS2_PLACEMENT_3D('',#3415,#2680,#2681);
#2147=AXIS2_PLACEMENT_3D('',#3416,#2682,#2683);
#2148=AXIS2_PLACEMENT_3D('',#3418,#2684,#2685);
#2149=AXIS2_PLACEMENT_3D('',#3419,#2686,#2687);
#2150=AXIS2_PLACEMENT_3D('',#3420,#2688,#2689);
#2151=AXIS2_PLACEMENT_3D('',#3444,#2690,#2691);
#2152=AXIS2_PLACEMENT_3D('',#3445,#2692,#2693);
#2153=AXIS2_PLACEMENT_3D('',#3447,#2694,#2695);
#2154=AXIS2_PLACEMENT_3D('',#3448,#2696,#2697);
#2155=AXIS2_PLACEMENT_3D('',#3449,#2698,#2699);
#2156=AXIS2_PLACEMENT_3D('',#3473,#2700,#2701);
#2157=AXIS2_PLACEMENT_3D('',#3474,#2702,#2703);
#2158=AXIS2_PLACEMENT_3D('',#3476,#2704,#2705);
#2159=AXIS2_PLACEMENT_3D('',#3478,#2706,#2707);
#2160=AXIS2_PLACEMENT_3D('',#3479,#2708,#2709);
#2161=AXIS2_PLACEMENT_3D('',#3480,#2710,#2711);
#2162=AXIS2_PLACEMENT_3D('',#3504,#2712,#2713);
#2163=AXIS2_PLACEMENT_3D('',#3505,#2714,#2715);
#2164=AXIS2_PLACEMENT_3D('',#3507,#2716,#2717);
#2165=AXIS2_PLACEMENT_3D('',#3508,#2718,#2719);
#2166=AXIS2_PLACEMENT_3D('',#3509,#2720,#2721);
#2167=AXIS2_PLACEMENT_3D('',#3533,#2722,#2723);
#2168=AXIS2_PLACEMENT_3D('',#3534,#2724,#2725);
#2169=AXIS2_PLACEMENT_3D('',#3536,#2726,#2727);
#2170=AXIS2_PLACEMENT_3D('',#3537,#2728,#2729);
#2171=AXIS2_PLACEMENT_3D('',#3538,#2730,#2731);
#2172=AXIS2_PLACEMENT_3D('',#3562,#2732,#2733);
#2173=AXIS2_PLACEMENT_3D('',#3563,#2734,#2735);
#2174=AXIS2_PLACEMENT_3D('',#3565,#2736,#2737);
#2175=AXIS2_PLACEMENT_3D('',#3568,#2739,#2740);
#2176=AXIS2_PLACEMENT_3D('',#3592,#2741,#2742);
#2177=AXIS2_PLACEMENT_3D('',#3593,#2743,#2744);
#2178=AXIS2_PLACEMENT_3D('',#3594,#2745,#2746);
#2179=AXIS2_PLACEMENT_3D('',#3595,#2747,#2748);
#2180=AXIS2_PLACEMENT_3D('',#3596,#2749,#2750);
#2181=AXIS2_PLACEMENT_3D('',#3597,#2751,#2752);
#2182=AXIS2_PLACEMENT_3D('',#3598,#2753,#2754);
#2183=AXIS2_PLACEMENT_3D('',#3599,#2755,#2756);
#2184=AXIS2_PLACEMENT_3D('',#3600,#2757,#2758);
#2185=AXIS2_PLACEMENT_3D('',#3602,#2759,#2760);
#2186=AXIS2_PLACEMENT_3D('',#3604,#2761,#2762);
#2187=AXIS2_PLACEMENT_3D('',#3605,#2763,#2764);
#2188=AXIS2_PLACEMENT_3D('',#3607,#2765,#2766);
#2189=AXIS2_PLACEMENT_3D('',#3609,#2768,#2769);
#2190=AXIS2_PLACEMENT_3D('',#3611,#2770,#2771);
#2191=AXIS2_PLACEMENT_3D('',#3612,#2772,#2773);
#2192=AXIS2_PLACEMENT_3D('',#3614,#2775,#2776);
#2193=AXIS2_PLACEMENT_3D('',#3616,#2777,#2778);
#2194=AXIS2_PLACEMENT_3D('',#3618,#2779,#2780);
#2195=AXIS2_PLACEMENT_3D('',#3619,#2781,#2782);
#2196=AXIS2_PLACEMENT_3D('',#3621,#2783,#2784);
#2197=AXIS2_PLACEMENT_3D('',#3623,#2786,#2787);
#2198=AXIS2_PLACEMENT_3D('',#3625,#2788,#2789);
#2199=AXIS2_PLACEMENT_3D('',#3626,#2790,#2791);
#2200=AXIS2_PLACEMENT_3D('',#3628,#2793,#2794);
#2201=AXIS2_PLACEMENT_3D('',#3629,#2795,#2796);
#2202=AXIS2_PLACEMENT_3D('',#3630,#2797,#2798);
#2203=AXIS2_PLACEMENT_3D('',#3631,#2799,#2800);
#2204=AXIS2_PLACEMENT_3D('',#3632,#2801,#2802);
#2205=AXIS2_PLACEMENT_3D('',#3633,#2803,#2804);
#2206=AXIS2_PLACEMENT_3D('',#3634,#2805,#2806);
#2207=AXIS2_PLACEMENT_3D('',#3636,#2807,#2808);
#2208=AXIS2_PLACEMENT_3D('',#3639,#2810,#2811);
#2209=AXIS2_PLACEMENT_3D('',#3640,#2812,#2813);
#2210=AXIS2_PLACEMENT_3D('',#3642,#2814,#2815);
#2211=AXIS2_PLACEMENT_3D('',#3645,#2817,#2818);
#2212=AXIS2_PLACEMENT_3D('',#3646,#2819,#2820);
#2213=AXIS2_PLACEMENT_3D('',#3647,#2821,#2822);
#2214=AXIS2_PLACEMENT_3D('',#3648,#2823,#2824);
#2215=AXIS2_PLACEMENT_3D('',#3649,#2825,#2826);
#2216=AXIS2_PLACEMENT_3D('',#3650,#2827,#2828);
#2217=AXIS2_PLACEMENT_3D('',#3651,#2829,#2830);
#2218=AXIS2_PLACEMENT_3D('',#3652,#2831,#2832);
#2219=AXIS2_PLACEMENT_3D('',#3653,#2833,#2834);
#2220=AXIS2_PLACEMENT_3D('',#3654,#2835,#2836);
#2221=DIRECTION('axis',(0.,0.,1.));
#2222=DIRECTION('refdir',(1.,0.,0.));
#2223=DIRECTION('axis',(0.,0.,1.));
#2224=DIRECTION('refdir',(1.,0.,0.));
#2225=DIRECTION('axis',(0.,0.,1.));
#2226=DIRECTION('refdir',(1.,0.,0.));
#2227=DIRECTION('center_axis',(0.,0.,1.));
#2228=DIRECTION('ref_axis',(1.,0.,0.));
#2229=DIRECTION('center_axis',(0.,0.,1.));
#2230=DIRECTION('ref_axis',(1.,0.,0.));
#2231=DIRECTION('',(0.,0.,1.));
#2232=DIRECTION('center_axis',(0.,0.,-1.));
#2233=DIRECTION('ref_axis',(1.,0.,0.));
#2234=DIRECTION('center_axis',(0.,0.,1.));
#2235=DIRECTION('ref_axis',(1.,0.,0.));
#2236=DIRECTION('center_axis',(0.,0.,1.));
#2237=DIRECTION('ref_axis',(1.,0.,0.));
#2238=DIRECTION('',(0.,0.,1.));
#2239=DIRECTION('center_axis',(0.,0.,-1.));
#2240=DIRECTION('ref_axis',(1.,0.,0.));
#2241=DIRECTION('center_axis',(0.,0.,1.));
#2242=DIRECTION('ref_axis',(1.,0.,0.));
#2243=DIRECTION('center_axis',(0.,0.,1.));
#2244=DIRECTION('ref_axis',(1.,0.,0.));
#2245=DIRECTION('',(0.,0.,1.));
#2246=DIRECTION('center_axis',(0.,0.,-1.));
#2247=DIRECTION('ref_axis',(1.,0.,0.));
#2248=DIRECTION('center_axis',(0.,0.,1.));
#2249=DIRECTION('ref_axis',(1.,0.,0.));
#2250=DIRECTION('center_axis',(0.,0.,1.));
#2251=DIRECTION('ref_axis',(1.,0.,0.));
#2252=DIRECTION('',(0.,0.,1.));
#2253=DIRECTION('center_axis',(0.,0.,-1.));
#2254=DIRECTION('ref_axis',(1.,0.,0.));
#2255=DIRECTION('center_axis',(0.,1.,0.));
#2256=DIRECTION('ref_axis',(1.,0.,0.));
#2257=DIRECTION('center_axis',(0.,1.,0.));
#2258=DIRECTION('ref_axis',(1.,0.,0.));
#2259=DIRECTION('',(0.,1.,0.));
#2260=DIRECTION('center_axis',(0.,-1.,0.));
#2261=DIRECTION('ref_axis',(1.,0.,0.));
#2262=DIRECTION('center_axis',(0.,1.,0.));
#2263=DIRECTION('ref_axis',(1.,0.,0.));
#2264=DIRECTION('center_axis',(0.,1.,0.));
#2265=DIRECTION('ref_axis',(1.,0.,0.));
#2266=DIRECTION('',(0.,1.,0.));
#2267=DIRECTION('center_axis',(0.,-1.,0.));
#2268=DIRECTION('ref_axis',(1.,0.,0.));
#2269=DIRECTION('center_axis',(0.,1.,0.));
#2270=DIRECTION('ref_axis',(1.,0.,0.));
#2271=DIRECTION('',(-1.,0.,0.));
#2272=DIRECTION('',(0.,0.,1.));
#2273=DIRECTION('',(-1.,0.,0.));
#2274=DIRECTION('',(0.,0.,-1.));
#2275=DIRECTION('center_axis',(1.,0.,0.));
#2276=DIRECTION('ref_axis',(0.,0.,-1.));
#2277=DIRECTION('',(0.,-1.,0.));
#2278=DIRECTION('',(0.,0.,-1.));
#2279=DIRECTION('',(0.,1.,0.));
#2280=DIRECTION('center_axis',(-1.,0.,0.));
#2281=DIRECTION('ref_axis',(0.,0.,1.));
#2282=DIRECTION('',(0.,1.,0.));
#2283=DIRECTION('',(0.,1.,0.));
#2284=DIRECTION('',(0.,0.,1.));
#2285=DIRECTION('center_axis',(0.,0.,1.));
#2286=DIRECTION('ref_axis',(1.,0.,0.));
#2287=DIRECTION('',(1.,0.,0.));
#2288=DIRECTION('center_axis',(0.,1.,0.));
#2289=DIRECTION('ref_axis',(0.,0.,1.));
#2290=DIRECTION('',(1.,0.,0.));
#2291=DIRECTION('center_axis',(0.,1.,0.));
#2292=DIRECTION('ref_axis',(1.,0.,0.));
#2293=DIRECTION('',(-1.,0.,0.));
#2294=DIRECTION('',(0.,0.,1.));
#2295=DIRECTION('',(-1.,0.,0.));
#2296=DIRECTION('',(0.,0.,-1.));
#2297=DIRECTION('center_axis',(1.,0.,0.));
#2298=DIRECTION('ref_axis',(0.,0.,-1.));
#2299=DIRECTION('',(0.,-1.,0.));
#2300=DIRECTION('',(0.,0.,-1.));
#2301=DIRECTION('',(0.,1.,0.));
#2302=DIRECTION('center_axis',(-1.,0.,0.));
#2303=DIRECTION('ref_axis',(0.,0.,1.));
#2304=DIRECTION('',(0.,1.,0.));
#2305=DIRECTION('',(0.,1.,0.));
#2306=DIRECTION('',(0.,0.,1.));
#2307=DIRECTION('center_axis',(0.,0.,1.));
#2308=DIRECTION('ref_axis',(1.,0.,0.));
#2309=DIRECTION('',(1.,0.,0.));
#2310=DIRECTION('center_axis',(0.,1.,0.));
#2311=DIRECTION('ref_axis',(0.,0.,1.));
#2312=DIRECTION('',(1.,0.,0.));
#2313=DIRECTION('center_axis',(0.,1.,0.));
#2314=DIRECTION('ref_axis',(-1.,0.,0.));
#2315=DIRECTION('',(-1.,0.,0.));
#2316=DIRECTION('',(0.,0.,1.));
#2317=DIRECTION('',(-1.,0.,0.));
#2318=DIRECTION('',(0.,0.,1.));
#2319=DIRECTION('center_axis',(1.,0.,0.));
#2320=DIRECTION('ref_axis',(0.,1.,0.));
#2321=DIRECTION('',(0.,1.,0.));
#2322=DIRECTION('',(0.,1.,0.));
#2323=DIRECTION('',(0.,0.,1.));
#2324=DIRECTION('center_axis',(0.,-1.,0.));
#2325=DIRECTION('ref_axis',(1.,0.,0.));
#2326=DIRECTION('',(1.,0.,0.));
#2327=DIRECTION('',(1.,0.,0.));
#2328=DIRECTION('',(0.,0.,1.));
#2329=DIRECTION('center_axis',(-1.,0.,0.));
#2330=DIRECTION('ref_axis',(0.,-1.,0.));
#2331=DIRECTION('',(0.,-1.,0.));
#2332=DIRECTION('',(0.,-1.,0.));
#2333=DIRECTION('center_axis',(0.,0.,1.));
#2334=DIRECTION('ref_axis',(1.,0.,0.));
#2335=DIRECTION('center_axis',(0.,0.,1.));
#2336=DIRECTION('ref_axis',(1.,0.,0.));
#2337=DIRECTION('axis',(0.,0.,1.));
#2338=DIRECTION('refdir',(1.,0.,0.));
#2339=DIRECTION('center_axis',(0.,1.,0.));
#2340=DIRECTION('ref_axis',(1.,0.,0.));
#2341=DIRECTION('center_axis',(0.,1.,0.));
#2342=DIRECTION('ref_axis',(1.,0.,0.));
#2343=DIRECTION('',(0.,1.,0.));
#2344=DIRECTION('center_axis',(0.,-1.,0.));
#2345=DIRECTION('ref_axis',(1.,0.,0.));
#2346=DIRECTION('center_axis',(0.,1.,0.));
#2347=DIRECTION('ref_axis',(1.,0.,0.));
#2348=DIRECTION('center_axis',(0.,1.,0.));
#2349=DIRECTION('ref_axis',(1.,0.,0.));
#2350=DIRECTION('center_axis',(0.,1.,0.));
#2351=DIRECTION('ref_axis',(1.,0.,0.));
#2352=DIRECTION('center_axis',(0.,1.,0.));
#2353=DIRECTION('ref_axis',(1.,0.,0.));
#2354=DIRECTION('center_axis',(0.,1.,0.));
#2355=DIRECTION('ref_axis',(1.,0.,0.));
#2356=DIRECTION('',(0.,-1.,0.));
#2357=DIRECTION('center_axis',(0.,1.,0.));
#2358=DIRECTION('ref_axis',(1.,0.,0.));
#2359=DIRECTION('center_axis',(0.,1.,0.));
#2360=DIRECTION('ref_axis',(1.,0.,0.));
#2361=DIRECTION('center_axis',(0.,1.,0.));
#2362=DIRECTION('ref_axis',(1.,0.,0.));
#2363=DIRECTION('center_axis',(0.,1.,0.));
#2364=DIRECTION('ref_axis',(1.,0.,0.));
#2365=DIRECTION('',(0.,-1.,0.));
#2366=DIRECTION('center_axis',(0.,1.,0.));
#2367=DIRECTION('ref_axis',(1.,0.,0.));
#2368=DIRECTION('axis',(0.,0.,1.));
#2369=DIRECTION('refdir',(1.,0.,0.));
#2370=DIRECTION('center_axis',(0.,1.,0.));
#2371=DIRECTION('ref_axis',(1.,0.,0.));
#2372=DIRECTION('center_axis',(0.,-1.,0.));
#2373=DIRECTION('ref_axis',(1.,0.,0.));
#2374=DIRECTION('',(0.,-1.,0.));
#2375=DIRECTION('center_axis',(0.,-1.,0.));
#2376=DIRECTION('ref_axis',(1.,0.,0.));
#2377=DIRECTION('center_axis',(0.,1.,0.));
#2378=DIRECTION('ref_axis',(1.,0.,0.));
#2379=DIRECTION('center_axis',(0.,1.,0.));
#2380=DIRECTION('ref_axis',(1.,0.,0.));
#2381=DIRECTION('',(0.,-1.,0.));
#2382=DIRECTION('center_axis',(0.,1.,0.));
#2383=DIRECTION('ref_axis',(1.,0.,0.));
#2384=DIRECTION('center_axis',(0.,1.,0.));
#2385=DIRECTION('ref_axis',(1.,0.,0.));
#2386=DIRECTION('center_axis',(0.,1.,0.));
#2387=DIRECTION('ref_axis',(1.,0.,0.));
#2388=DIRECTION('axis',(0.,0.,1.));
#2389=DIRECTION('refdir',(1.,0.,0.));
#2390=DIRECTION('center_axis',(0.,1.,0.));
#2391=DIRECTION('ref_axis',(1.,0.,0.));
#2392=DIRECTION('center_axis',(0.,-1.,0.));
#2393=DIRECTION('ref_axis',(1.,0.,0.));
#2394=DIRECTION('',(0.,-1.,0.));
#2395=DIRECTION('center_axis',(0.,-1.,0.));
#2396=DIRECTION('ref_axis',(1.,0.,0.));
#2397=DIRECTION('center_axis',(0.,1.,0.));
#2398=DIRECTION('ref_axis',(1.,0.,0.));
#2399=DIRECTION('center_axis',(0.,1.,0.));
#2400=DIRECTION('ref_axis',(1.,0.,0.));
#2401=DIRECTION('',(0.,-1.,0.));
#2402=DIRECTION('center_axis',(0.,1.,0.));
#2403=DIRECTION('ref_axis',(1.,0.,0.));
#2404=DIRECTION('center_axis',(0.,1.,0.));
#2405=DIRECTION('ref_axis',(1.,0.,0.));
#2406=DIRECTION('center_axis',(0.,1.,0.));
#2407=DIRECTION('ref_axis',(1.,0.,0.));
#2408=DIRECTION('axis',(0.,0.,1.));
#2409=DIRECTION('refdir',(1.,0.,0.));
#2410=DIRECTION('center_axis',(0.866025403784439,0.,-0.5));
#2411=DIRECTION('ref_axis',(0.5,0.,0.866025403784439));
#2412=DIRECTION('',(-0.5,0.,-0.866025403784439));
#2413=DIRECTION('',(0.,-1.,0.));
#2414=DIRECTION('',(0.5,0.,0.866025403784439));
#2415=DIRECTION('',(0.,-1.,0.));
#2416=DIRECTION('center_axis',(1.60246890531964E-16,0.,-1.));
#2417=DIRECTION('ref_axis',(1.,0.,1.60246890531964E-16));
#2418=DIRECTION('',(-1.,0.,-1.60246890531964E-16));
#2419=DIRECTION('',(0.,-1.,0.));
#2420=DIRECTION('',(1.,0.,1.60246890531964E-16));
#2421=DIRECTION('center_axis',(-0.866025403784439,0.,-0.5));
#2422=DIRECTION('ref_axis',(0.5,0.,-0.866025403784439));
#2423=DIRECTION('',(-0.5,0.,0.866025403784439));
#2424=DIRECTION('',(0.,-1.,0.));
#2425=DIRECTION('',(0.5,0.,-0.866025403784439));
#2426=DIRECTION('center_axis',(-0.866025403784439,0.,0.5));
#2427=DIRECTION('ref_axis',(-0.5,0.,-0.866025403784439));
#2428=DIRECTION('',(0.5,0.,0.866025403784439));
#2429=DIRECTION('',(0.,-1.,0.));
#2430=DIRECTION('',(-0.5,0.,-0.866025403784439));
#2431=DIRECTION('center_axis',(-1.60246890531964E-16,0.,1.));
#2432=DIRECTION('ref_axis',(-1.,0.,-1.60246890531964E-16));
#2433=DIRECTION('',(1.,0.,1.60246890531964E-16));
#2434=DIRECTION('',(0.,-1.,0.));
#2435=DIRECTION('',(-1.,0.,-1.60246890531964E-16));
#2436=DIRECTION('center_axis',(0.866025403784439,0.,0.5));
#2437=DIRECTION('ref_axis',(-0.5,0.,0.866025403784439));
#2438=DIRECTION('',(0.5,0.,-0.866025403784439));
#2439=DIRECTION('',(-0.5,0.,0.866025403784439));
#2440=DIRECTION('center_axis',(0.,1.,0.));
#2441=DIRECTION('ref_axis',(1.,0.,0.));
#2442=DIRECTION('center_axis',(0.,-1.,0.));
#2443=DIRECTION('ref_axis',(0.,0.,-1.));
#2444=DIRECTION('center_axis',(0.,1.,0.));
#2445=DIRECTION('ref_axis',(1.,0.,0.));
#2446=DIRECTION('center_axis',(0.,1.,0.));
#2447=DIRECTION('ref_axis',(1.,0.,0.));
#2448=DIRECTION('center_axis',(0.,1.,0.));
#2449=DIRECTION('ref_axis',(0.,0.,1.));
#2450=DIRECTION('center_axis',(0.,-1.,0.));
#2451=DIRECTION('ref_axis',(1.,0.,0.));
#2452=DIRECTION('center_axis',(0.,-1.,0.));
#2453=DIRECTION('ref_axis',(1.,0.,0.));
#2454=DIRECTION('center_axis',(0.,-1.,0.));
#2455=DIRECTION('ref_axis',(1.,0.,0.));
#2456=DIRECTION('',(0.707106781186547,0.707106781186548,8.65956056235493E-17));
#2457=DIRECTION('center_axis',(0.,-1.,0.));
#2458=DIRECTION('ref_axis',(1.,0.,0.));
#2459=DIRECTION('center_axis',(0.,-1.,0.));
#2460=DIRECTION('ref_axis',(1.,0.,0.));
#2461=DIRECTION('',(0.,1.,0.));
#2462=DIRECTION('center_axis',(0.,1.,0.));
#2463=DIRECTION('ref_axis',(1.,0.,0.));
#2464=DIRECTION('center_axis',(0.,-1.,0.));
#2465=DIRECTION('ref_axis',(1.,0.,0.));
#2466=DIRECTION('',(-0.707106781186547,0.707106781186548,-8.65956056235493E-17));
#2467=DIRECTION('center_axis',(0.,-1.,0.));
#2468=DIRECTION('ref_axis',(0.,0.,-1.));
#2469=DIRECTION('center_axis',(0.,-1.,0.));
#2470=DIRECTION('ref_axis',(1.,0.,0.));
#2471=DIRECTION('center_axis',(0.,1.,0.));
#2472=DIRECTION('ref_axis',(1.,0.,0.));
#2473=DIRECTION('center_axis',(0.,1.,0.));
#2474=DIRECTION('ref_axis',(1.,0.,0.));
#2475=DIRECTION('',(-0.447213595499958,0.894427190999916,-5.47678698264203E-17));
#2476=DIRECTION('center_axis',(0.,-1.,0.));
#2477=DIRECTION('ref_axis',(1.,0.,0.));
#2478=DIRECTION('',(0.,1.,0.));
#2479=DIRECTION('',(0.,0.,1.));
#2480=DIRECTION('',(1.,0.,0.));
#2481=DIRECTION('',(0.,0.,1.));
#2482=DIRECTION('',(1.,0.,0.));
#2483=DIRECTION('',(0.,0.,1.));
#2484=DIRECTION('',(1.,0.,0.));
#2485=DIRECTION('',(0.,0.,1.));
#2486=DIRECTION('',(1.,0.,0.));
#2487=DIRECTION('',(0.,0.,1.));
#2488=DIRECTION('',(1.,0.,0.));
#2489=DIRECTION('',(0.,0.,1.));
#2490=DIRECTION('',(1.,0.,0.));
#2491=DIRECTION('axis',(0.,0.,1.));
#2492=DIRECTION('refdir',(1.,0.,0.));
#2493=DIRECTION('axis',(0.,0.,1.));
#2494=DIRECTION('refdir',(1.,0.,0.));
#2495=DIRECTION('center_axis',(0.,1.,0.));
#2496=DIRECTION('ref_axis',(1.,0.,0.));
#2497=DIRECTION('center_axis',(0.,1.,0.));
#2498=DIRECTION('ref_axis',(1.,0.,0.));
#2499=DIRECTION('',(0.,1.,0.));
#2500=DIRECTION('center_axis',(0.,-1.,0.));
#2501=DIRECTION('ref_axis',(1.,0.,0.));
#2502=DIRECTION('center_axis',(0.,1.,0.));
#2503=DIRECTION('ref_axis',(1.,0.,0.));
#2504=DIRECTION('center_axis',(0.,1.,0.));
#2505=DIRECTION('ref_axis',(1.,0.,0.));
#2506=DIRECTION('center_axis',(0.,1.,0.));
#2507=DIRECTION('ref_axis',(1.,0.,0.));
#2508=DIRECTION('center_axis',(0.,1.,0.));
#2509=DIRECTION('ref_axis',(1.,0.,0.));
#2510=DIRECTION('',(0.,1.,0.));
#2511=DIRECTION('center_axis',(0.,1.,0.));
#2512=DIRECTION('ref_axis',(1.,0.,0.));
#2513=DIRECTION('center_axis',(0.,1.,0.));
#2514=DIRECTION('ref_axis',(1.,0.,0.));
#2515=DIRECTION('center_axis',(0.,-1.,0.));
#2516=DIRECTION('ref_axis',(1.,0.,0.));
#2517=DIRECTION('center_axis',(0.,1.,0.));
#2518=DIRECTION('ref_axis',(1.,0.,0.));
#2519=DIRECTION('',(0.,-1.,0.));
#2520=DIRECTION('center_axis',(0.,1.,0.));
#2521=DIRECTION('ref_axis',(1.,0.,0.));
#2522=DIRECTION('center_axis',(0.,1.,0.));
#2523=DIRECTION('ref_axis',(1.,0.,0.));
#2524=DIRECTION('',(0.,-1.,0.));
#2525=DIRECTION('center_axis',(0.,1.,0.));
#2526=DIRECTION('ref_axis',(1.,0.,0.));
#2527=DIRECTION('center_axis',(0.,1.,0.));
#2528=DIRECTION('ref_axis',(1.,0.,0.));
#2529=DIRECTION('center_axis',(0.,1.,0.));
#2530=DIRECTION('ref_axis',(1.,0.,0.));
#2531=DIRECTION('axis',(0.,0.,1.));
#2532=DIRECTION('refdir',(1.,0.,0.));
#2533=DIRECTION('axis',(0.,0.,1.));
#2534=DIRECTION('refdir',(1.,0.,0.));
#2535=DIRECTION('center_axis',(0.,-1.,0.));
#2536=DIRECTION('ref_axis',(0.,0.,-1.));
#2537=DIRECTION('center_axis',(0.,-1.,0.));
#2538=DIRECTION('ref_axis',(1.,0.,0.));
#2539=DIRECTION('center_axis',(0.,-1.,0.));
#2540=DIRECTION('ref_axis',(1.,0.,0.));
#2541=DIRECTION('center_axis',(1.,0.,1.22464679914735E-16));
#2542=DIRECTION('ref_axis',(-1.22464679914735E-16,0.,1.));
#2543=DIRECTION('center_axis',(0.,1.,0.));
#2544=DIRECTION('ref_axis',(1.,0.,0.));
#2545=DIRECTION('center_axis',(0.,1.,0.));
#2546=DIRECTION('ref_axis',(1.,0.,0.));
#2547=DIRECTION('center_axis',(0.,-1.,0.));
#2548=DIRECTION('ref_axis',(1.,0.,0.));
#2549=DIRECTION('',(0.,1.,0.));
#2550=DIRECTION('center_axis',(0.,-1.,0.));
#2551=DIRECTION('ref_axis',(1.,0.,0.));
#2552=DIRECTION('center_axis',(0.,-1.,0.));
#2553=DIRECTION('ref_axis',(1.,0.,0.));
#2554=DIRECTION('center_axis',(0.,-1.,0.));
#2555=DIRECTION('ref_axis',(1.,0.,0.));
#2556=DIRECTION('',(0.,1.,0.));
#2557=DIRECTION('center_axis',(0.,-1.,0.));
#2558=DIRECTION('ref_axis',(1.,0.,0.));
#2559=DIRECTION('center_axis',(0.,1.,0.));
#2560=DIRECTION('ref_axis',(1.,0.,0.));
#2561=DIRECTION('',(-0.707106781186548,0.707106781186547,-8.65956056235493E-17));
#2562=DIRECTION('center_axis',(0.,-1.,0.));
#2563=DIRECTION('ref_axis',(1.,0.,0.));
#2564=DIRECTION('center_axis',(0.,1.,0.));
#2565=DIRECTION('ref_axis',(0.,0.,1.));
#2566=DIRECTION('center_axis',(0.,-1.,0.));
#2567=DIRECTION('ref_axis',(1.,0.,0.));
#2568=DIRECTION('center_axis',(0.,-1.,0.));
#2569=DIRECTION('ref_axis',(1.,0.,0.));
#2570=DIRECTION('',(0.,1.,0.));
#2571=DIRECTION('center_axis',(0.,-1.,0.));
#2572=DIRECTION('ref_axis',(0.,0.,-1.));
#2573=DIRECTION('center_axis',(0.,-1.,0.));
#2574=DIRECTION('ref_axis',(1.,0.,0.));
#2575=DIRECTION('center_axis',(0.,-1.,0.));
#2576=DIRECTION('ref_axis',(1.,0.,0.));
#2577=DIRECTION('',(0.707106781186548,0.707106781186547,8.65956056235493E-17));
#2578=DIRECTION('axis',(0.,0.,1.));
#2579=DIRECTION('refdir',(1.,0.,0.));
#2580=DIRECTION('center_axis',(0.,-1.,0.));
#2581=DIRECTION('ref_axis',(0.,0.,-1.));
#2582=DIRECTION('center_axis',(0.,-1.,0.));
#2583=DIRECTION('ref_axis',(1.,0.,0.));
#2584=DIRECTION('center_axis',(0.,-1.,0.));
#2585=DIRECTION('ref_axis',(1.,0.,0.));
#2586=DIRECTION('center_axis',(1.,0.,1.22464679914735E-16));
#2587=DIRECTION('ref_axis',(-1.22464679914735E-16,0.,1.));
#2588=DIRECTION('center_axis',(0.,1.,0.));
#2589=DIRECTION('ref_axis',(1.,0.,0.));
#2590=DIRECTION('center_axis',(0.,1.,0.));
#2591=DIRECTION('ref_axis',(1.,0.,0.));
#2592=DIRECTION('center_axis',(0.,-1.,0.));
#2593=DIRECTION('ref_axis',(1.,0.,0.));
#2594=DIRECTION('center_axis',(0.,-1.,0.));
#2595=DIRECTION('ref_axis',(1.,0.,0.));
#2596=DIRECTION('',(0.,1.,0.));
#2597=DIRECTION('center_axis',(0.,1.,0.));
#2598=DIRECTION('ref_axis',(0.,0.,1.));
#2599=DIRECTION('center_axis',(0.,-1.,0.));
#2600=DIRECTION('ref_axis',(1.,0.,0.));
#2601=DIRECTION('center_axis',(0.,-1.,0.));
#2602=DIRECTION('ref_axis',(1.,0.,0.));
#2603=DIRECTION('center_axis',(0.,-1.,0.));
#2604=DIRECTION('ref_axis',(1.,0.,0.));
#2605=DIRECTION('center_axis',(0.,-1.,0.));
#2606=DIRECTION('ref_axis',(1.,0.,0.));
#2607=DIRECTION('',(0.707106781186548,0.707106781186547,8.65956056235494E-17));
#2608=DIRECTION('center_axis',(0.,-1.,0.));
#2609=DIRECTION('ref_axis',(1.,0.,0.));
#2610=DIRECTION('center_axis',(0.,-1.,0.));
#2611=DIRECTION('ref_axis',(1.,0.,0.));
#2612=DIRECTION('',(0.,1.,0.));
#2613=DIRECTION('center_axis',(0.,1.,0.));
#2614=DIRECTION('ref_axis',(1.,0.,0.));
#2615=DIRECTION('center_axis',(0.,-1.,0.));
#2616=DIRECTION('ref_axis',(1.,0.,0.));
#2617=DIRECTION('',(-0.707106781186548,0.707106781186547,-8.65956056235494E-17));
#2618=DIRECTION('center_axis',(0.,-1.,0.));
#2619=DIRECTION('ref_axis',(0.,0.,-1.));
#2620=DIRECTION('center_axis',(0.,-1.,0.));
#2621=DIRECTION('ref_axis',(1.,0.,0.));
#2622=DIRECTION('',(0.,1.,0.));
#2623=DIRECTION('axis',(0.,0.,1.));
#2624=DIRECTION('refdir',(1.,0.,0.));
#2625=DIRECTION('center_axis',(0.,0.,1.));
#2626=DIRECTION('ref_axis',(1.,0.,0.));
#2627=DIRECTION('center_axis',(1.22464679914735E-16,-1.,0.));
#2628=DIRECTION('ref_axis',(-1.,-1.22464679914735E-16,0.));
#2629=DIRECTION('center_axis',(0.78183148246803,0.,0.623489801858733));
#2630=DIRECTION('ref_axis',(0.623489801858734,0.,-0.78183148246803));
#2631=DIRECTION('center_axis',(7.63554790147315E-17,-1.,-9.57467422477103E-17));
#2632=DIRECTION('ref_axis',(-0.623489801858734,-1.22464679914735E-16,0.78183148246803));
#2633=DIRECTION('center_axis',(0.974927912181824,0.,-0.222520933956314));
#2634=DIRECTION('ref_axis',(-0.222520933956314,0.,-0.974927912181824));
#2635=DIRECTION('center_axis',(-2.7250954951288E-17,-1.,-1.19394234705288E-16));
#2636=DIRECTION('ref_axis',(0.222520933956314,-1.22464679914735E-16,0.974927912181824));
#2637=DIRECTION('center_axis',(0.433883739117558,0.,-0.900968867902419));
#2638=DIRECTION('ref_axis',(-0.900968867902419,0.,-0.433883739117558));
#2639=DIRECTION('center_axis',(-1.10336864020811E-16,-1.,-5.31354332312403E-17));
#2640=DIRECTION('ref_axis',(0.900968867902419,-1.22464679914735E-16,0.433883739117558));
#2641=DIRECTION('center_axis',(-0.433883739117558,0.,-0.900968867902419));
#2642=DIRECTION('ref_axis',(-0.900968867902419,0.,0.433883739117558));
#2643=DIRECTION('center_axis',(-1.10336864020811E-16,-1.,5.31354332312403E-17));
#2644=DIRECTION('ref_axis',(0.900968867902419,-1.22464679914735E-16,-0.433883739117558));
#2645=DIRECTION('center_axis',(-0.974927912181824,0.,-0.222520933956314));
#2646=DIRECTION('ref_axis',(-0.222520933956315,0.,0.974927912181824));
#2647=DIRECTION('center_axis',(-2.7250954951288E-17,-1.,1.19394234705288E-16));
#2648=DIRECTION('ref_axis',(0.222520933956315,-1.22464679914735E-16,-0.974927912181824));
#2649=DIRECTION('center_axis',(-0.78183148246803,0.,0.623489801858734));
#2650=DIRECTION('ref_axis',(0.623489801858733,0.,0.78183148246803));
#2651=DIRECTION('center_axis',(7.63554790147315E-17,-1.,9.57467422477103E-17));
#2652=DIRECTION('ref_axis',(-0.623489801858733,-1.22464679914735E-16,-0.78183148246803));
#2653=DIRECTION('axis',(0.,0.,1.));
#2654=DIRECTION('refdir',(1.,0.,0.));
#2655=DIRECTION('center_axis',(0.,0.,1.));
#2656=DIRECTION('ref_axis',(1.,0.,0.));
#2657=DIRECTION('center_axis',(0.,-1.,0.));
#2658=DIRECTION('ref_axis',(0.,0.,-1.));
#2659=DIRECTION('center_axis',(0.,-1.,0.));
#2660=DIRECTION('ref_axis',(0.,0.,-1.));
#2661=DIRECTION('center_axis',(0.,1.,0.));
#2662=DIRECTION('ref_axis',(1.,0.,0.));
#2663=DIRECTION('center_axis',(0.,1.,0.));
#2664=DIRECTION('ref_axis',(1.,0.,0.));
#2665=DIRECTION('center_axis',(0.,1.,0.));
#2666=DIRECTION('ref_axis',(1.,0.,0.));
#2667=DIRECTION('center_axis',(0.,1.,0.));
#2668=DIRECTION('ref_axis',(1.,0.,0.));
#2669=DIRECTION('',(0.,-1.,0.));
#2670=DIRECTION('center_axis',(0.,-1.,0.));
#2671=DIRECTION('ref_axis',(1.,0.,0.));
#2672=DIRECTION('center_axis',(0.,1.,0.));
#2673=DIRECTION('ref_axis',(1.,0.,0.));
#2674=DIRECTION('center_axis',(0.,1.,0.));
#2675=DIRECTION('ref_axis',(1.,0.,0.));
#2676=DIRECTION('center_axis',(0.,1.,0.));
#2677=DIRECTION('ref_axis',(1.,0.,0.));
#2678=DIRECTION('center_axis',(0.,1.,0.));
#2679=DIRECTION('ref_axis',(1.,0.,0.));
#2680=DIRECTION('center_axis',(0.,1.,0.));
#2681=DIRECTION('ref_axis',(1.,0.,0.));
#2682=DIRECTION('center_axis',(0.,1.,0.));
#2683=DIRECTION('ref_axis',(1.,0.,0.));
#2684=DIRECTION('center_axis',(0.,-1.,0.));
#2685=DIRECTION('ref_axis',(1.,0.,0.));
#2686=DIRECTION('center_axis',(0.,-1.,0.));
#2687=DIRECTION('ref_axis',(0.,0.,-1.));
#2688=DIRECTION('center_axis',(8.96625347776458E-17,0.,1.));
#2689=DIRECTION('ref_axis',(1.,0.,0.));
#2690=DIRECTION('center_axis',(0.,-1.,0.));
#2691=DIRECTION('ref_axis',(0.,0.,-1.));
#2692=DIRECTION('center_axis',(0.,1.,0.));
#2693=DIRECTION('ref_axis',(1.,0.,0.));
#2694=DIRECTION('center_axis',(0.,-1.,0.));
#2695=DIRECTION('ref_axis',(1.,0.,0.));
#2696=DIRECTION('center_axis',(0.,-1.,0.));
#2697=DIRECTION('ref_axis',(0.,0.,-1.));
#2698=DIRECTION('center_axis',(0.,0.,1.));
#2699=DIRECTION('ref_axis',(1.,0.,0.));
#2700=DIRECTION('center_axis',(0.,-1.,0.));
#2701=DIRECTION('ref_axis',(0.,0.,-1.));
#2702=DIRECTION('center_axis',(0.,1.,0.));
#2703=DIRECTION('ref_axis',(1.,0.,0.));
#2704=DIRECTION('center_axis',(0.,-1.,0.));
#2705=DIRECTION('ref_axis',(1.,0.,0.));
#2706=DIRECTION('center_axis',(0.,-1.,0.));
#2707=DIRECTION('ref_axis',(1.,0.,0.));
#2708=DIRECTION('center_axis',(0.,-1.,0.));
#2709=DIRECTION('ref_axis',(0.,0.,-1.));
#2710=DIRECTION('center_axis',(0.,0.,1.));
#2711=DIRECTION('ref_axis',(1.,0.,0.));
#2712=DIRECTION('center_axis',(0.,-1.,0.));
#2713=DIRECTION('ref_axis',(0.,0.,-1.));
#2714=DIRECTION('center_axis',(0.,1.,0.));
#2715=DIRECTION('ref_axis',(1.,0.,0.));
#2716=DIRECTION('center_axis',(0.,-1.,0.));
#2717=DIRECTION('ref_axis',(1.,0.,0.));
#2718=DIRECTION('center_axis',(0.,-1.,0.));
#2719=DIRECTION('ref_axis',(0.,0.,-1.));
#2720=DIRECTION('center_axis',(8.96625347776458E-17,0.,1.));
#2721=DIRECTION('ref_axis',(1.,0.,0.));
#2722=DIRECTION('center_axis',(0.,-1.,0.));
#2723=DIRECTION('ref_axis',(0.,0.,-1.));
#2724=DIRECTION('center_axis',(0.,1.,0.));
#2725=DIRECTION('ref_axis',(1.,0.,0.));
#2726=DIRECTION('center_axis',(0.,-1.,0.));
#2727=DIRECTION('ref_axis',(1.,0.,0.));
#2728=DIRECTION('center_axis',(0.,-1.,0.));
#2729=DIRECTION('ref_axis',(0.,0.,-1.));
#2730=DIRECTION('center_axis',(0.,0.,1.));
#2731=DIRECTION('ref_axis',(1.,0.,0.));
#2732=DIRECTION('center_axis',(0.,-1.,0.));
#2733=DIRECTION('ref_axis',(0.,0.,-1.));
#2734=DIRECTION('center_axis',(0.,1.,0.));
#2735=DIRECTION('ref_axis',(1.,0.,0.));
#2736=DIRECTION('center_axis',(0.,1.,0.));
#2737=DIRECTION('ref_axis',(1.,0.,0.));
#2738=DIRECTION('',(0.,1.,0.));
#2739=DIRECTION('center_axis',(0.,-1.,0.));
#2740=DIRECTION('ref_axis',(1.,0.,0.));
#2741=DIRECTION('center_axis',(0.,-1.,0.));
#2742=DIRECTION('ref_axis',(1.,0.,0.));
#2743=DIRECTION('center_axis',(0.,1.,0.));
#2744=DIRECTION('ref_axis',(1.,0.,0.));
#2745=DIRECTION('center_axis',(0.,-1.,0.));
#2746=DIRECTION('ref_axis',(0.,0.,-1.));
#2747=DIRECTION('center_axis',(0.,0.,1.));
#2748=DIRECTION('ref_axis',(1.,0.,0.));
#2749=DIRECTION('center_axis',(0.,-1.,0.));
#2750=DIRECTION('ref_axis',(0.,0.,-1.));
#2751=DIRECTION('center_axis',(0.,-1.,0.));
#2752=DIRECTION('ref_axis',(-1.,0.,0.));
#2753=DIRECTION('center_axis',(0.,1.,0.));
#2754=DIRECTION('ref_axis',(1.,0.,0.));
#2755=DIRECTION('axis',(0.,0.,1.));
#2756=DIRECTION('refdir',(1.,0.,0.));
#2757=DIRECTION('center_axis',(0.,1.,0.));
#2758=DIRECTION('ref_axis',(0.,0.,1.));
#2759=DIRECTION('center_axis',(0.,-1.,0.));
#2760=DIRECTION('ref_axis',(1.,0.,0.));
#2761=DIRECTION('center_axis',(0.,-1.,0.));
#2762=DIRECTION('ref_axis',(1.,0.,0.));
#2763=DIRECTION('center_axis',(0.,-1.,0.));
#2764=DIRECTION('ref_axis',(1.,0.,0.));
#2765=DIRECTION('center_axis',(0.,-1.,0.));
#2766=DIRECTION('ref_axis',(1.,0.,0.));
#2767=DIRECTION('',(0.,1.,0.));
#2768=DIRECTION('center_axis',(0.,-1.,0.));
#2769=DIRECTION('ref_axis',(0.,0.,-1.));
#2770=DIRECTION('center_axis',(0.,-1.,0.));
#2771=DIRECTION('ref_axis',(1.,0.,0.));
#2772=DIRECTION('center_axis',(0.,-1.,0.));
#2773=DIRECTION('ref_axis',(1.,0.,0.));
#2774=DIRECTION('',(0.,1.,0.));
#2775=DIRECTION('center_axis',(0.,1.,0.));
#2776=DIRECTION('ref_axis',(0.,0.,1.));
#2777=DIRECTION('center_axis',(0.,-1.,0.));
#2778=DIRECTION('ref_axis',(1.,0.,0.));
#2779=DIRECTION('center_axis',(0.,-1.,0.));
#2780=DIRECTION('ref_axis',(1.,0.,0.));
#2781=DIRECTION('center_axis',(0.,-1.,0.));
#2782=DIRECTION('ref_axis',(1.,0.,0.));
#2783=DIRECTION('center_axis',(0.,-1.,0.));
#2784=DIRECTION('ref_axis',(1.,0.,0.));
#2785=DIRECTION('',(0.,1.,0.));
#2786=DIRECTION('center_axis',(0.,-1.,0.));
#2787=DIRECTION('ref_axis',(0.,0.,-1.));
#2788=DIRECTION('center_axis',(0.,-1.,0.));
#2789=DIRECTION('ref_axis',(1.,0.,0.));
#2790=DIRECTION('center_axis',(0.,-1.,0.));
#2791=DIRECTION('ref_axis',(1.,0.,0.));
#2792=DIRECTION('',(0.,1.,0.));
#2793=DIRECTION('',(0.,0.,1.));
#2794=DIRECTION('',(1.,0.,0.));
#2795=DIRECTION('',(0.,0.,1.));
#2796=DIRECTION('',(1.,0.,0.));
#2797=DIRECTION('',(0.,0.,1.));
#2798=DIRECTION('',(1.,0.,0.));
#2799=DIRECTION('',(0.,0.,1.));
#2800=DIRECTION('',(1.,0.,0.));
#2801=DIRECTION('',(0.,0.,1.));
#2802=DIRECTION('',(1.,0.,0.));
#2803=DIRECTION('axis',(0.,0.,1.));
#2804=DIRECTION('refdir',(1.,0.,0.));
#2805=DIRECTION('center_axis',(0.,1.,0.));
#2806=DIRECTION('ref_axis',(1.,0.,0.));
#2807=DIRECTION('center_axis',(0.,-1.,0.));
#2808=DIRECTION('ref_axis',(1.,0.,0.));
#2809=DIRECTION('',(0.,-1.,0.));
#2810=DIRECTION('center_axis',(0.,-1.,0.));
#2811=DIRECTION('ref_axis',(1.,0.,0.));
#2812=DIRECTION('center_axis',(0.,1.,0.));
#2813=DIRECTION('ref_axis',(1.,0.,0.));
#2814=DIRECTION('center_axis',(0.,1.,0.));
#2815=DIRECTION('ref_axis',(1.,0.,0.));
#2816=DIRECTION('',(0.,-1.,0.));
#2817=DIRECTION('center_axis',(0.,1.,0.));
#2818=DIRECTION('ref_axis',(1.,0.,0.));
#2819=DIRECTION('center_axis',(0.,1.,0.));
#2820=DIRECTION('ref_axis',(1.,0.,0.));
#2821=DIRECTION('center_axis',(0.,1.,0.));
#2822=DIRECTION('ref_axis',(1.,0.,0.));
#2823=DIRECTION('',(0.,0.,1.));
#2824=DIRECTION('',(1.,0.,0.));
#2825=DIRECTION('',(0.,0.,1.));
#2826=DIRECTION('',(1.,0.,0.));
#2827=DIRECTION('',(0.,0.,1.));
#2828=DIRECTION('',(1.,0.,0.));
#2829=DIRECTION('',(0.,0.,1.));
#2830=DIRECTION('',(1.,0.,0.));
#2831=DIRECTION('',(0.,0.,1.));
#2832=DIRECTION('',(1.,0.,0.));
#2833=DIRECTION('',(0.,0.,1.));
#2834=DIRECTION('',(1.,0.,0.));
#2835=DIRECTION('',(0.,0.,1.));
#2836=DIRECTION('',(1.,0.,0.));
#2837=CARTESIAN_POINT('',(0.,0.,0.));
#2838=CARTESIAN_POINT('',(0.,0.,0.));
#2839=CARTESIAN_POINT('',(0.,0.,0.));
#2840=CARTESIAN_POINT('Origin',(2.4,-1.6,-0.1));
#2841=CARTESIAN_POINT('',(2.125,-1.6,-0.3));
#2842=CARTESIAN_POINT('Origin',(2.4,-1.6,-0.3));
#2843=CARTESIAN_POINT('',(2.125,-1.6,0.6));
#2844=CARTESIAN_POINT('',(2.125,-1.6,-0.1));
#2845=CARTESIAN_POINT('Origin',(2.4,-1.6,0.6));
#2846=CARTESIAN_POINT('Origin',(-2.4,1.6,-0.1));
#2847=CARTESIAN_POINT('',(-2.675,1.6,-0.3));
#2848=CARTESIAN_POINT('Origin',(-2.4,1.6,-0.3));
#2849=CARTESIAN_POINT('',(-2.675,1.6,0.6));
#2850=CARTESIAN_POINT('',(-2.675,1.6,-0.1));
#2851=CARTESIAN_POINT('Origin',(-2.4,1.6,0.6));
#2852=CARTESIAN_POINT('Origin',(-2.4,-1.6,-0.1));
#2853=CARTESIAN_POINT('',(-2.675,-1.6,-0.3));
#2854=CARTESIAN_POINT('Origin',(-2.4,-1.6,-0.3));
#2855=CARTESIAN_POINT('',(-2.675,-1.6,0.6));
#2856=CARTESIAN_POINT('',(-2.675,-1.6,-0.1));
#2857=CARTESIAN_POINT('Origin',(-2.4,-1.6,0.6));
#2858=CARTESIAN_POINT('Origin',(2.4,1.6,-0.1));
#2859=CARTESIAN_POINT('',(2.125,1.6,-0.3));
#2860=CARTESIAN_POINT('Origin',(2.4,1.6,-0.3));
#2861=CARTESIAN_POINT('',(2.125,1.6,0.6));
#2862=CARTESIAN_POINT('',(2.125,1.6,-0.1));
#2863=CARTESIAN_POINT('Origin',(2.4,1.6,0.6));
#2864=CARTESIAN_POINT('Origin',(0.,-2.1,3.5));
#2865=CARTESIAN_POINT('',(-0.6,-2.,3.5));
#2866=CARTESIAN_POINT('Origin',(0.,-2.,3.5));
#2867=CARTESIAN_POINT('',(-0.6,-1.5,3.5));
#2868=CARTESIAN_POINT('',(-0.6,-2.1,3.5));
#2869=CARTESIAN_POINT('Origin',(0.,-1.5,3.5));
#2870=CARTESIAN_POINT('Origin',(0.,-2.1,3.5));
#2871=CARTESIAN_POINT('',(-0.6,1.5,3.5));
#2872=CARTESIAN_POINT('Origin',(0.,1.5,3.5));
#2873=CARTESIAN_POINT('',(-0.6,2.,3.5));
#2874=CARTESIAN_POINT('',(-0.6,-2.1,3.5));
#2875=CARTESIAN_POINT('Origin',(0.,2.,3.5));
#2876=CARTESIAN_POINT('Origin',(0.,1.5,2.6));
#2877=CARTESIAN_POINT('',(1.4,1.5,0.6));
#2878=CARTESIAN_POINT('',(-1.4,1.5,0.600000000000001));
#2879=CARTESIAN_POINT('',(0.,1.5,0.6));
#2880=CARTESIAN_POINT('',(1.4,1.5,4.7));
#2881=CARTESIAN_POINT('',(1.4,1.5,0.5));
#2882=CARTESIAN_POINT('',(-1.4,1.5,4.7));
#2883=CARTESIAN_POINT('',(1.4,1.5,4.7));
#2884=CARTESIAN_POINT('',(-1.4,1.5,4.7));
#2885=CARTESIAN_POINT('Origin',(1.4,1.5,4.7));
#2886=CARTESIAN_POINT('',(1.4,2.,0.6));
#2887=CARTESIAN_POINT('',(1.4,0.75,0.6));
#2888=CARTESIAN_POINT('',(1.4,2.,4.7));
#2889=CARTESIAN_POINT('',(1.4,2.,0.5));
#2890=CARTESIAN_POINT('',(1.4,1.5,4.7));
#2891=CARTESIAN_POINT('Origin',(-1.4,1.5,0.5));
#2892=CARTESIAN_POINT('',(-1.4,2.,0.600000000000001));
#2893=CARTESIAN_POINT('',(-1.4,0.75,0.6));
#2894=CARTESIAN_POINT('',(-1.4,2.,4.7));
#2895=CARTESIAN_POINT('',(-1.4,1.5,4.7));
#2896=CARTESIAN_POINT('',(-1.4,2.,4.7));
#2897=CARTESIAN_POINT('Origin',(-1.4,1.5,4.7));
#2898=CARTESIAN_POINT('',(1.4,2.,4.7));
#2899=CARTESIAN_POINT('Origin',(0.,2.,2.6));
#2900=CARTESIAN_POINT('',(0.,2.,0.6));
#2901=CARTESIAN_POINT('Origin',(0.,-2.,2.6));
#2902=CARTESIAN_POINT('',(1.4,-2.,0.6));
#2903=CARTESIAN_POINT('',(-1.4,-2.,0.600000000000001));
#2904=CARTESIAN_POINT('',(0.,-2.,0.6));
#2905=CARTESIAN_POINT('',(1.4,-2.,4.7));
#2906=CARTESIAN_POINT('',(1.4,-2.,0.5));
#2907=CARTESIAN_POINT('',(-1.4,-2.,4.7));
#2908=CARTESIAN_POINT('',(1.4,-2.,4.7));
#2909=CARTESIAN_POINT('',(-1.4,-2.,4.7));
#2910=CARTESIAN_POINT('Origin',(1.4,-2.,4.7));
#2911=CARTESIAN_POINT('',(1.4,-1.5,0.6));
#2912=CARTESIAN_POINT('',(1.4,-1.,0.6));
#2913=CARTESIAN_POINT('',(1.4,-1.5,4.7));
#2914=CARTESIAN_POINT('',(1.4,-1.5,0.5));
#2915=CARTESIAN_POINT('',(1.4,-2.,4.7));
#2916=CARTESIAN_POINT('Origin',(-1.4,-2.,0.5));
#2917=CARTESIAN_POINT('',(-1.4,-1.5,0.600000000000001));
#2918=CARTESIAN_POINT('',(-1.4,-1.,0.6));
#2919=CARTESIAN_POINT('',(-1.4,-1.5,4.7));
#2920=CARTESIAN_POINT('',(-1.4,-2.,4.7));
#2921=CARTESIAN_POINT('',(-1.4,-1.5,4.7));
#2922=CARTESIAN_POINT('Origin',(-1.4,-2.,4.7));
#2923=CARTESIAN_POINT('',(1.4,-1.5,4.7));
#2924=CARTESIAN_POINT('Origin',(0.,-1.5,2.6));
#2925=CARTESIAN_POINT('',(0.,-1.5,0.6));
#2926=CARTESIAN_POINT('Origin',(3.,2.5,0.));
#2927=CARTESIAN_POINT('',(3.,2.5,-0.3));
#2928=CARTESIAN_POINT('',(-3.,2.5,-0.3));
#2929=CARTESIAN_POINT('',(1.5,2.5,-0.3));
#2930=CARTESIAN_POINT('',(-3.,2.5,0.6));
#2931=CARTESIAN_POINT('',(-3.,2.5,0.));
#2932=CARTESIAN_POINT('',(3.,2.5,0.6));
#2933=CARTESIAN_POINT('',(3.,2.5,0.6));
#2934=CARTESIAN_POINT('',(3.,2.5,0.));
#2935=CARTESIAN_POINT('Origin',(3.,-2.5,0.));
#2936=CARTESIAN_POINT('',(3.,-2.5,-0.3));
#2937=CARTESIAN_POINT('',(3.,-1.25,-0.3));
#2938=CARTESIAN_POINT('',(3.,-2.5,0.6));
#2939=CARTESIAN_POINT('',(3.,-2.5,0.6));
#2940=CARTESIAN_POINT('',(3.,-2.5,0.));
#2941=CARTESIAN_POINT('Origin',(-3.,-2.5,0.));
#2942=CARTESIAN_POINT('',(-3.,-2.5,-0.3));
#2943=CARTESIAN_POINT('',(-1.5,-2.5,-0.3));
#2944=CARTESIAN_POINT('',(-3.,-2.5,0.6));
#2945=CARTESIAN_POINT('',(-3.,-2.5,0.6));
#2946=CARTESIAN_POINT('',(-3.,-2.5,0.));
#2947=CARTESIAN_POINT('Origin',(-3.,2.5,0.));
#2948=CARTESIAN_POINT('',(-3.,1.25,-0.3));
#2949=CARTESIAN_POINT('',(-3.,2.5,0.6));
#2950=CARTESIAN_POINT('Origin',(0.,0.,0.6));
#2951=CARTESIAN_POINT('Origin',(0.,0.,-0.3));
#2952=CARTESIAN_POINT('',(0.,0.,0.));
#2953=CARTESIAN_POINT('Origin',(0.,0.9,3.5));
#2954=CARTESIAN_POINT('',(-0.165,0.9,3.5));
#2955=CARTESIAN_POINT('Origin',(0.,0.9,3.5));
#2956=CARTESIAN_POINT('',(-0.165,2.,3.5));
#2957=CARTESIAN_POINT('',(-0.165,0.9,3.5));
#2958=CARTESIAN_POINT('Origin',(0.,2.,3.5));
#2959=CARTESIAN_POINT('Origin',(0.,0.9,3.5));
#2960=CARTESIAN_POINT('Origin',(0.,-2.,3.5));
#2961=CARTESIAN_POINT('',(-0.9,-2.,3.5));
#2962=CARTESIAN_POINT('Origin',(0.,-2.,3.5));
#2963=CARTESIAN_POINT('',(-0.6,-2.,3.5));
#2964=CARTESIAN_POINT('Origin',(0.,-2.,3.5));
#2965=CARTESIAN_POINT('Origin',(0.,-2.4,3.5));
#2966=CARTESIAN_POINT('',(-0.9,-2.4,3.5));
#2967=CARTESIAN_POINT('',(-0.9,-2.4,3.5));
#2968=CARTESIAN_POINT('Origin',(0.,-2.4,3.5));
#2969=CARTESIAN_POINT('Origin',(0.,-2.4,3.5));
#2970=CARTESIAN_POINT('Origin',(0.,-2.,3.5));
#2971=CARTESIAN_POINT('',(-0.6,2.,3.5));
#2972=CARTESIAN_POINT('Origin',(0.,2.,3.5));
#2973=CARTESIAN_POINT('',(-0.6,-2.,3.5));
#2974=CARTESIAN_POINT('Origin',(0.,2.,3.5));
#2975=CARTESIAN_POINT('',(0.,0.,0.));
#2976=CARTESIAN_POINT('Origin',(0.,4.5,10.));
#2977=CARTESIAN_POINT('',(-0.605,4.9,10.));
#2978=CARTESIAN_POINT('Origin',(0.,4.9,10.));
#2979=CARTESIAN_POINT('',(-0.605,4.5,10.));
#2980=CARTESIAN_POINT('',(-0.605,4.5,10.));
#2981=CARTESIAN_POINT('Origin',(0.,4.5,10.));
#2982=CARTESIAN_POINT('Origin',(0.,4.5,10.));
#2983=CARTESIAN_POINT('',(-0.8,4.9,10.));
#2984=CARTESIAN_POINT('Origin',(0.,4.9,10.));
#2985=CARTESIAN_POINT('',(-0.8,4.5,10.));
#2986=CARTESIAN_POINT('',(-0.8,4.5,10.));
#2987=CARTESIAN_POINT('Origin',(0.,4.5,10.));
#2988=CARTESIAN_POINT('Origin',(0.,4.9,10.));
#2989=CARTESIAN_POINT('Origin',(0.,4.5,10.));
#2990=CARTESIAN_POINT('',(0.,0.,0.));
#2991=CARTESIAN_POINT('Origin',(0.,2.2,4.));
#2992=CARTESIAN_POINT('',(-0.225,2.4,4.));
#2993=CARTESIAN_POINT('Origin',(0.,2.4,4.));
#2994=CARTESIAN_POINT('',(-0.225,2.2,4.));
#2995=CARTESIAN_POINT('',(-0.225,2.2,4.));
#2996=CARTESIAN_POINT('Origin',(0.,2.2,4.));
#2997=CARTESIAN_POINT('Origin',(0.,2.2,4.));
#2998=CARTESIAN_POINT('',(-0.8,2.4,4.));
#2999=CARTESIAN_POINT('Origin',(0.,2.4,4.));
#3000=CARTESIAN_POINT('',(-0.8,2.2,4.));
#3001=CARTESIAN_POINT('',(-0.8,2.2,4.));
#3002=CARTESIAN_POINT('Origin',(0.,2.2,4.));
#3003=CARTESIAN_POINT('Origin',(0.,2.4,4.));
#3004=CARTESIAN_POINT('Origin',(0.,2.2,4.));
#3005=CARTESIAN_POINT('',(0.,0.,0.));
#3006=CARTESIAN_POINT('Origin',(0.0866025403784439,-0.4,-0.15));
#3007=CARTESIAN_POINT('',(0.173205080756888,-0.4,0.));
#3008=CARTESIAN_POINT('',(0.0866025403784439,-0.4,-0.15));
#3009=CARTESIAN_POINT('',(0.173205080756888,-0.4,0.));
#3010=CARTESIAN_POINT('',(0.0866025403784439,-0.64,-0.15));
#3011=CARTESIAN_POINT('',(0.0866025403784439,-0.4,-0.15));
#3012=CARTESIAN_POINT('',(0.173205080756888,-0.64,0.));
#3013=CARTESIAN_POINT('',(0.173205080756888,-0.64,0.));
#3014=CARTESIAN_POINT('',(0.173205080756888,-0.4,0.));
#3015=CARTESIAN_POINT('Origin',(-0.0866025403784438,-0.4,-0.15));
#3016=CARTESIAN_POINT('',(-0.0866025403784438,-0.4,-0.15));
#3017=CARTESIAN_POINT('',(0.0866025403784439,-0.4,-0.15));
#3018=CARTESIAN_POINT('',(-0.0866025403784438,-0.64,-0.15));
#3019=CARTESIAN_POINT('',(-0.0866025403784438,-0.4,-0.15));
#3020=CARTESIAN_POINT('',(0.0866025403784439,-0.64,-0.15));
#3021=CARTESIAN_POINT('Origin',(-0.173205080756888,-0.4,-2.77555756156289E-17));
#3022=CARTESIAN_POINT('',(-0.173205080756888,-0.4,-2.12115047744981E-17));
#3023=CARTESIAN_POINT('',(-0.0866025403784438,-0.4,-0.15));
#3024=CARTESIAN_POINT('',(-0.173205080756888,-0.64,-2.77555756156289E-17));
#3025=CARTESIAN_POINT('',(-0.173205080756888,-0.4,-2.12115047744981E-17));
#3026=CARTESIAN_POINT('',(-0.0866025403784438,-0.64,-0.15));
#3027=CARTESIAN_POINT('Origin',(-0.0866025403784439,-0.4,0.15));
#3028=CARTESIAN_POINT('',(-0.0866025403784439,-0.4,0.15));
#3029=CARTESIAN_POINT('',(-0.173205080756888,-0.4,-2.12115047744981E-17));
#3030=CARTESIAN_POINT('',(-0.0866025403784439,-0.64,0.15));
#3031=CARTESIAN_POINT('',(-0.0866025403784439,-0.4,0.15));
#3032=CARTESIAN_POINT('',(-0.173205080756888,-0.64,-2.12115047744981E-17));
#3033=CARTESIAN_POINT('Origin',(0.0866025403784439,-0.4,0.15));
#3034=CARTESIAN_POINT('',(0.0866025403784439,-0.4,0.15));
#3035=CARTESIAN_POINT('',(-0.0866025403784439,-0.4,0.15));
#3036=CARTESIAN_POINT('',(0.0866025403784439,-0.64,0.15));
#3037=CARTESIAN_POINT('',(0.0866025403784439,-0.4,0.15));
#3038=CARTESIAN_POINT('',(-0.0866025403784439,-0.64,0.15));
#3039=CARTESIAN_POINT('Origin',(0.173205080756888,-0.4,0.));
#3040=CARTESIAN_POINT('',(0.0866025403784439,-0.4,0.15));
#3041=CARTESIAN_POINT('',(0.0866025403784439,-0.64,0.15));
#3042=CARTESIAN_POINT('Origin',(0.,-0.4,-2.77555756156289E-17));
#3043=CARTESIAN_POINT('Origin',(0.,-0.64,-2.77555756156289E-17));
#3044=CARTESIAN_POINT('Origin',(0.,-1.,0.));
#3045=CARTESIAN_POINT('',(-0.1954,-1.,2.39295984553393E-17));
#3046=CARTESIAN_POINT('Origin',(0.,-1.,0.));
#3047=CARTESIAN_POINT('Origin',(0.3,0.4,0.));
#3048=CARTESIAN_POINT('',(-0.3,0.4,-3.67394039744206E-17));
#3049=CARTESIAN_POINT('Origin',(0.,0.4,0.));
#3050=CARTESIAN_POINT('Origin',(0.,0.375,0.));
#3051=CARTESIAN_POINT('',(-0.35,0.35,-4.28626379701573E-17));
#3052=CARTESIAN_POINT('Origin',(0.,0.35,0.));
#3053=CARTESIAN_POINT('',(-0.325,0.375,-3.9801020972289E-17));
#3054=CARTESIAN_POINT('Origin',(0.,0.19,0.));
#3055=CARTESIAN_POINT('',(-0.35,0.03,-4.28626379701574E-17));
#3056=CARTESIAN_POINT('Origin',(0.,0.03,0.));
#3057=CARTESIAN_POINT('',(-0.35,0.19,-4.28626379701574E-17));
#3058=CARTESIAN_POINT('Origin',(0.,0.0149999999999999,0.));
#3059=CARTESIAN_POINT('',(-0.32,-3.29597460435593E-17,-3.91886975727153E-17));
#3060=CARTESIAN_POINT('Origin',(0.,0.,0.));
#3061=CARTESIAN_POINT('',(-0.335,0.0149999999999999,-4.10256677714363E-17));
#3062=CARTESIAN_POINT('Origin',(0.22,0.,0.));
#3063=CARTESIAN_POINT('',(-0.22,-6.93889390390723E-18,-2.69422295812418E-17));
#3064=CARTESIAN_POINT('Origin',(0.,0.,0.));
#3065=CARTESIAN_POINT('Origin',(0.,-0.02,0.));
#3066=CARTESIAN_POINT('',(-0.1954,-0.0492,2.39295984553393E-17));
#3067=CARTESIAN_POINT('Origin',(0.,-0.0492,0.));
#3068=CARTESIAN_POINT('',(-0.21,-0.02,-2.57175827820944E-17));
#3069=CARTESIAN_POINT('Origin',(0.,-0.8,0.));
#3070=CARTESIAN_POINT('',(-0.1954,-0.8,-2.39295984553393E-17));
#3071=CARTESIAN_POINT('',(0.,0.,0.));
#3072=CARTESIAN_POINT('',(0.,0.,0.));
#3073=CARTESIAN_POINT('',(0.,-3.4,-6.5));
#3074=CARTESIAN_POINT('',(0.,-6.,-6.5));
#3075=CARTESIAN_POINT('',(0.,-0.2,-0.5));
#3076=CARTESIAN_POINT('',(0.,2.2,3.5));
#3077=CARTESIAN_POINT('',(0.,0.,0.));
#3078=CARTESIAN_POINT('',(0.,0.,0.));
#3079=CARTESIAN_POINT('Origin',(0.,0.1,3.5));
#3080=CARTESIAN_POINT('',(-1.6,0.1,3.5));
#3081=CARTESIAN_POINT('Origin',(0.,0.1,3.5));
#3082=CARTESIAN_POINT('',(-1.6,1.3,3.5));
#3083=CARTESIAN_POINT('',(-1.6,0.1,3.5));
#3084=CARTESIAN_POINT('Origin',(0.,1.3,3.5));
#3085=CARTESIAN_POINT('Origin',(0.,0.1,3.5));
#3086=CARTESIAN_POINT('',(-0.62,0.1,3.5));
#3087=CARTESIAN_POINT('Origin',(0.,0.1,3.5));
#3088=CARTESIAN_POINT('Origin',(0.,-1.4,3.5));
#3089=CARTESIAN_POINT('',(-1.6,-1.3,3.5));
#3090=CARTESIAN_POINT('Origin',(0.,-1.3,3.5));
#3091=CARTESIAN_POINT('',(-1.6,-0.1,3.5));
#3092=CARTESIAN_POINT('',(-1.6,-1.4,3.5));
#3093=CARTESIAN_POINT('Origin',(0.,-0.1,3.5));
#3094=CARTESIAN_POINT('Origin',(0.,-0.1,3.5));
#3095=CARTESIAN_POINT('',(-0.62,-0.1,3.5));
#3096=CARTESIAN_POINT('Origin',(0.,-0.1,3.5));
#3097=CARTESIAN_POINT('Origin',(0.,-1.3,3.5));
#3098=CARTESIAN_POINT('',(-0.62,-1.3,3.5));
#3099=CARTESIAN_POINT('Origin',(0.,-1.3,3.5));
#3100=CARTESIAN_POINT('',(-2.5,1.3,3.5));
#3101=CARTESIAN_POINT('Origin',(0.,1.3,3.5));
#3102=CARTESIAN_POINT('',(-2.5,-1.3,3.5));
#3103=CARTESIAN_POINT('',(-2.5,-1.3,3.5));
#3104=CARTESIAN_POINT('Origin',(0.,-1.3,3.5));
#3105=CARTESIAN_POINT('Origin',(0.,1.3,3.5));
#3106=CARTESIAN_POINT('Origin',(0.,-1.3,3.5));
#3107=CARTESIAN_POINT('',(0.,0.,0.));
#3108=CARTESIAN_POINT('',(0.,0.,0.));
#3109=CARTESIAN_POINT('Origin',(0.,0.,0.));
#3110=CARTESIAN_POINT('',(-1.070235,-0.308121667383195,-1.31065986708547E-16));
#3111=CARTESIAN_POINT('',(-1.31065986708547E-16,-0.308121667383195,1.070235));
#3112=CARTESIAN_POINT('Origin',(0.,-0.308121667383195,0.));
#3113=CARTESIAN_POINT('Origin',(0.,-0.308121667383195,0.));
#3114=CARTESIAN_POINT('',(-1.31065986708547E-16,0.308121667383195,1.070235));
#3115=CARTESIAN_POINT('Origin',(-1.34711147906209E-16,0.,1.1));
#3116=CARTESIAN_POINT('',(-1.070235,0.308121667383195,1.31065986708547E-16));
#3117=CARTESIAN_POINT('Origin',(0.,0.308121667383195,0.));
#3118=CARTESIAN_POINT('Origin',(0.,0.308121667383195,0.));
#3119=CARTESIAN_POINT('Origin',(0.,0.,0.));
#3120=CARTESIAN_POINT('',(-1.070235,0.5,-1.31065986708547E-16));
#3121=CARTESIAN_POINT('',(-1.070235,0.,-1.31065986708547E-16));
#3122=CARTESIAN_POINT('Origin',(0.,0.5,0.));
#3123=CARTESIAN_POINT('Origin',(0.,0.,0.));
#3124=CARTESIAN_POINT('',(-0.6,-0.44,-7.34788079488412E-17));
#3125=CARTESIAN_POINT('Origin',(0.,-0.44,0.));
#3126=CARTESIAN_POINT('',(-0.6,0.44,-7.34788079488412E-17));
#3127=CARTESIAN_POINT('',(-0.6,0.,-7.34788079488412E-17));
#3128=CARTESIAN_POINT('Origin',(0.,0.44,0.));
#3129=CARTESIAN_POINT('Origin',(0.,0.47,0.));
#3130=CARTESIAN_POINT('',(-0.66,0.5,-8.08266887437253E-17));
#3131=CARTESIAN_POINT('',(-0.63,0.47,-7.71527483462832E-17));
#3132=CARTESIAN_POINT('Origin',(0.,0.5,0.));
#3133=CARTESIAN_POINT('Origin',(1.070235,0.5,0.));
#3134=CARTESIAN_POINT('Origin',(0.,0.,0.));
#3135=CARTESIAN_POINT('',(-1.070235,-0.5,-1.31065986708547E-16));
#3136=CARTESIAN_POINT('Origin',(0.,-0.5,0.));
#3137=CARTESIAN_POINT('',(-1.070235,0.,-1.31065986708547E-16));
#3138=CARTESIAN_POINT('Origin',(0.66,-0.5,0.));
#3139=CARTESIAN_POINT('',(-0.66,-0.5,-8.08266887437253E-17));
#3140=CARTESIAN_POINT('Origin',(0.,-0.5,0.));
#3141=CARTESIAN_POINT('Origin',(0.,-0.47,0.));
#3142=CARTESIAN_POINT('',(-0.63,-0.47,-7.71527483462832E-17));
#3143=CARTESIAN_POINT('',(0.,0.,0.));
#3144=CARTESIAN_POINT('Origin',(0.,0.,0.));
#3145=CARTESIAN_POINT('',(-1.129765,0.308121667383195,-1.38356309103871E-16));
#3146=CARTESIAN_POINT('',(-1.38356309103871E-16,0.308121667383195,1.129765));
#3147=CARTESIAN_POINT('Origin',(0.,0.308121667383195,0.));
#3148=CARTESIAN_POINT('Origin',(0.,0.308121667383195,0.));
#3149=CARTESIAN_POINT('',(-1.38356309103871E-16,-0.308121667383195,1.129765));
#3150=CARTESIAN_POINT('Origin',(-1.34711147906209E-16,0.,1.1));
#3151=CARTESIAN_POINT('',(-1.129765,-0.308121667383195,1.38356309103871E-16));
#3152=CARTESIAN_POINT('Origin',(0.,-0.308121667383195,0.));
#3153=CARTESIAN_POINT('Origin',(0.,-0.308121667383195,0.));
#3154=CARTESIAN_POINT('Origin',(0.,0.,0.));
#3155=CARTESIAN_POINT('',(-1.129765,-0.5,-1.38356309103871E-16));
#3156=CARTESIAN_POINT('Origin',(0.,-0.5,0.));
#3157=CARTESIAN_POINT('',(-1.129765,0.,-1.38356309103871E-16));
#3158=CARTESIAN_POINT('Origin',(1.54,0.5,0.));
#3159=CARTESIAN_POINT('',(-1.54,0.5,-1.88595607068692E-16));
#3160=CARTESIAN_POINT('Origin',(0.,0.5,0.));
#3161=CARTESIAN_POINT('',(-1.129765,0.5,-1.38356309103871E-16));
#3162=CARTESIAN_POINT('Origin',(0.,0.5,0.));
#3163=CARTESIAN_POINT('Origin',(0.,0.47,0.));
#3164=CARTESIAN_POINT('',(-1.6,0.44,-1.95943487863577E-16));
#3165=CARTESIAN_POINT('Origin',(0.,0.44,0.));
#3166=CARTESIAN_POINT('',(-1.57,0.47,-1.92269547466134E-16));
#3167=CARTESIAN_POINT('Origin',(0.,0.,0.));
#3168=CARTESIAN_POINT('',(-1.6,-0.44,-1.95943487863577E-16));
#3169=CARTESIAN_POINT('Origin',(0.,-0.44,0.));
#3170=CARTESIAN_POINT('',(-1.6,0.,-1.95943487863577E-16));
#3171=CARTESIAN_POINT('Origin',(0.,-0.47,0.));
#3172=CARTESIAN_POINT('',(-1.54,-0.5,-1.88595607068692E-16));
#3173=CARTESIAN_POINT('Origin',(0.,-0.5,0.));
#3174=CARTESIAN_POINT('',(-1.57,-0.47,-1.92269547466134E-16));
#3175=CARTESIAN_POINT('Origin',(1.129765,-0.5,0.));
#3176=CARTESIAN_POINT('Origin',(0.,0.,0.));
#3177=CARTESIAN_POINT('',(-1.129765,0.,-1.38356309103871E-16));
#3178=CARTESIAN_POINT('',(0.,0.,0.));
#3179=CARTESIAN_POINT('Origin',(1.1,0.,0.));
#3180=CARTESIAN_POINT('',(1.1,-2.23201749654651E-33,0.29765));
#3181=CARTESIAN_POINT('',(1.1,-2.23201749654651E-33,-0.29765));
#3182=CARTESIAN_POINT('Origin',(1.1,0.,0.));
#3183=CARTESIAN_POINT('Origin',(0.685838782044607,0.,-0.860014630714833));
#3184=CARTESIAN_POINT('',(0.918550922801216,-5.31350540756609E-33,-0.674432891191581));
#3185=CARTESIAN_POINT('',(0.453126641287998,8.49470414473068E-34,-1.04559637023808));
#3186=CARTESIAN_POINT('Origin',(0.685838782044607,0.,-0.860014630714833));
#3187=CARTESIAN_POINT('Origin',(-0.244773027351946,0.,-1.07242070340001));
#3188=CARTESIAN_POINT('',(0.0454142657089739,-2.23201749654651E-33,-1.1386540593921));
#3189=CARTESIAN_POINT('',(-0.534960320412865,-2.23201749654651E-33,-1.00618734740791));
#3190=CARTESIAN_POINT('Origin',(-0.244773027351946,0.,-1.07242070340001));
#3191=CARTESIAN_POINT('Origin',(-0.991065754692661,0.,-0.477272113029314));
#3192=CARTESIAN_POINT('',(-0.86192025974432,8.49470414473067E-34,-0.745445496560469));
#3193=CARTESIAN_POINT('',(-1.120211249641,-5.31350540756609E-33,-0.209098729498159));
#3194=CARTESIAN_POINT('Origin',(-0.991065754692661,0.,-0.477272113029314));
#3195=CARTESIAN_POINT('Origin',(-0.991065754692661,0.,0.477272113029314));
#3196=CARTESIAN_POINT('',(-1.120211249641,-2.23201749654651E-33,0.209098729498159));
#3197=CARTESIAN_POINT('',(-0.86192025974432,-2.23201749654651E-33,0.745445496560469));
#3198=CARTESIAN_POINT('Origin',(-0.991065754692661,0.,0.477272113029314));
#3199=CARTESIAN_POINT('Origin',(-0.244773027351946,0.,1.07242070340001));
#3200=CARTESIAN_POINT('',(-0.534960320412866,-2.23201749654651E-33,1.00618734740791));
#3201=CARTESIAN_POINT('',(0.0454142657089737,-2.23201749654651E-33,1.1386540593921));
#3202=CARTESIAN_POINT('Origin',(-0.244773027351946,0.,1.07242070340001));
#3203=CARTESIAN_POINT('Origin',(0.685838782044607,0.,0.860014630714833));
#3204=CARTESIAN_POINT('',(0.453126641287998,-2.23201749654651E-33,1.04559637023808));
#3205=CARTESIAN_POINT('',(0.918550922801216,-2.23201749654651E-33,0.674432891191581));
#3206=CARTESIAN_POINT('Origin',(0.685838782044607,0.,0.860014630714833));
#3207=CARTESIAN_POINT('',(0.,0.,0.));
#3208=CARTESIAN_POINT('Origin',(0.685838782044607,0.,0.860014630714833));
#3209=CARTESIAN_POINT('',(0.413083465285518,-0.05953,0.993751811093549));
#3210=CARTESIAN_POINT('',(0.876916659919095,-0.05953,0.623857181492959));
#3211=CARTESIAN_POINT('Ctrl Pts',(0.413083465285518,-0.05953,0.993751811093549));
#3212=CARTESIAN_POINT('Ctrl Pts',(0.419070565453383,-0.0925528133349865,
0.991263089003441));
#3213=CARTESIAN_POINT('Ctrl Pts',(0.430199341854858,-0.124911173756694,
0.986608710139579));
#3214=CARTESIAN_POINT('Ctrl Pts',(0.457978755888596,-0.177924977804098,
0.973971221090534));
#3215=CARTESIAN_POINT('Ctrl Pts',(0.473077587363685,-0.199697230012983,
0.966820759530997));
#3216=CARTESIAN_POINT('Ctrl Pts',(0.507057380724533,-0.237895043532788,
0.949440676105255));
#3217=CARTESIAN_POINT('Ctrl Pts',(0.525933334162555,-0.254319232363049,
0.939198248544428));
#3218=CARTESIAN_POINT('Ctrl Pts',(0.564362943424238,-0.28018331644634,0.916597376014514));
#3219=CARTESIAN_POINT('Ctrl Pts',(0.585840553788742,-0.29104845371857,0.903141581680914));
#3220=CARTESIAN_POINT('Ctrl Pts',(0.629305439856167,-0.30527573347708,0.873412008702649));
#3221=CARTESIAN_POINT('Ctrl Pts',(0.651278921914856,-0.308638795020976,
0.857118508332695));
#3222=CARTESIAN_POINT('Ctrl Pts',(0.690705563850638,-0.308638795020976,
0.825676810575914));
#3223=CARTESIAN_POINT('Ctrl Pts',(0.711480111898423,-0.30527573347708,0.807879894508811));
#3224=CARTESIAN_POINT('Ctrl Pts',(0.750136149454208,-0.29104845371857,0.772120216227122));
#3225=CARTESIAN_POINT('Ctrl Pts',(0.768033796848072,-0.28018331644634,0.754175290318038));
#3226=CARTESIAN_POINT('Ctrl Pts',(0.798619410861634,-0.254319232363049,
0.721738358858166));
#3227=CARTESIAN_POINT('Ctrl Pts',(0.812805334167529,-0.237895043532788,
0.705614819529209));
#3228=CARTESIAN_POINT('Ctrl Pts',(0.837310877969633,-0.199697230012983,
0.676354402927683));
#3229=CARTESIAN_POINT('Ctrl Pts',(0.847641868610495,-0.177924977804098,
0.663225258065736));
#3230=CARTESIAN_POINT('Ctrl Pts',(0.866144010579847,-0.124911173756694,
0.638954437806245));
#3231=CARTESIAN_POINT('Ctrl Pts',(0.873158080166742,-0.0925528133349865,
0.62914037979579));
#3232=CARTESIAN_POINT('Ctrl Pts',(0.876916659919095,-0.05953,0.623857181492959));
#3233=CARTESIAN_POINT('',(0.437601487681057,-0.05953,1.03511272300331));
#3234=CARTESIAN_POINT('Origin',(0.685838782044607,-0.05953,0.860014630714833));
#3235=CARTESIAN_POINT('',(0.911784794170997,-0.05953,0.656964154625313));
#3236=CARTESIAN_POINT('Ctrl Pts',(0.911784794170998,-0.0595300000000001,
0.656964154625312));
#3237=CARTESIAN_POINT('Ctrl Pts',(0.909827729890942,-0.0762225747374255,
0.659680317203144));
#3238=CARTESIAN_POINT('Ctrl Pts',(0.907004864562642,-0.0928409665394228,
0.663576540841106));
#3239=CARTESIAN_POINT('Ctrl Pts',(0.895234408667242,-0.144299303100741,
0.679480524217551));
#3240=CARTESIAN_POINT('Ctrl Pts',(0.882797231409153,-0.177024326825049,
0.695831250979106));
#3241=CARTESIAN_POINT('Ctrl Pts',(0.854332839576145,-0.227269801620064,
0.73042219438957));
#3242=CARTESIAN_POINT('Ctrl Pts',(0.834863020612702,-0.251265615809407,
0.752807465209441));
#3243=CARTESIAN_POINT('Ctrl Pts',(0.800439809856111,-0.279889827963178,
0.789147407129766));
#3244=CARTESIAN_POINT('Ctrl Pts',(0.781998747691871,-0.290879136862659,
0.80756613568454));
#3245=CARTESIAN_POINT('Ctrl Pts',(0.742239891936898,-0.305251990234487,
0.844254137480382));
#3246=CARTESIAN_POINT('Ctrl Pts',(0.720906778729541,-0.308638795020976,
0.862505527716294));
#3247=CARTESIAN_POINT('Ctrl Pts',(0.680463863683392,-0.308638795020976,
0.894757676234429));
#3248=CARTESIAN_POINT('Ctrl Pts',(0.657923009631182,-0.305251990234488,
0.91149460735272));
#3249=CARTESIAN_POINT('Ctrl Pts',(0.613307674922609,-0.290879136862659,
0.942092777160053));
#3250=CARTESIAN_POINT('Ctrl Pts',(0.591247219971725,-0.279889827963178,
0.955972930713954));
#3251=CARTESIAN_POINT('Ctrl Pts',(0.548158511259202,-0.251265615809407,
0.981446681891443));
#3252=CARTESIAN_POINT('Ctrl Pts',(0.522002043615455,-0.227269801620063,
0.995447160474328));
#3253=CARTESIAN_POINT('Ctrl Pts',(0.481944444320713,-0.177024326825049,
1.01550068154148));
#3254=CARTESIAN_POINT('Ctrl Pts',(0.463236132117164,-0.14429930310074,1.0239876538093));
#3255=CARTESIAN_POINT('Ctrl Pts',(0.445111721969657,-0.0928409665394226,
1.03192403056628));
#3256=CARTESIAN_POINT('Ctrl Pts',(0.440685038163619,-0.0762225747374254,
1.03380912944435));
#3257=CARTESIAN_POINT('Ctrl Pts',(0.437601487681056,-0.05953,1.03511272300331));
#3258=CARTESIAN_POINT('Origin',(0.685838782044607,-0.05953,0.860014630714833));
#3259=CARTESIAN_POINT('Origin',(0.,-0.208355,0.));
#3260=CARTESIAN_POINT('',(0.0548532617164168,-0.05953,1.12247250791415));
#3261=CARTESIAN_POINT('Origin',(0.,-0.05953,0.));
#3262=CARTESIAN_POINT('',(-0.536443649899848,-0.05953,0.987512846410683));
#3263=CARTESIAN_POINT('Ctrl Pts',(0.0548532617164173,-0.0595300000000001,
1.12247250791414));
#3264=CARTESIAN_POINT('Ctrl Pts',(0.05150947068137,-0.0762225747374254,
1.12263591311425));
#3265=CARTESIAN_POINT('Ctrl Pts',(0.0467032526342597,-0.0928409665394227,
1.12285816383385));
#3266=CARTESIAN_POINT('Ctrl Pts',(0.0269302585198975,-0.144299303100741,
1.12357162229597));
#3267=CARTESIAN_POINT('Ctrl Pts',(0.006392292392153,-0.177024326825049,
1.12404235695137));
#3268=CARTESIAN_POINT('Ctrl Pts',(-0.0383992541984087,-0.227269801620063,
1.12335509974011));
#3269=CARTESIAN_POINT('Ctrl Pts',(-0.0680399972366993,-0.251265615809407,
1.12208997038458));
#3270=CARTESIAN_POINT('Ctrl Pts',(-0.117914228755037,-0.279889827963178,
1.1178344036749));
#3271=CARTESIAN_POINT('Ctrl Pts',(-0.14381238480104,-0.290879136862659,
1.11490049012186));
#3272=CARTESIAN_POINT('Ctrl Pts',(-0.19728546073067,-0.305251990234488,
1.10669035995599));
#3273=CARTESIAN_POINT('Ctrl Pts',(-0.224855950742601,-0.308638795020976,
1.10139101611326));
#3274=CARTESIAN_POINT('Ctrl Pts',(-0.275287440920027,-0.308638795020976,
1.0898803575765));
#3275=CARTESIAN_POINT('Ctrl Pts',(-0.302426893214945,-0.305251990234488,
1.08269251410343));
#3276=CARTESIAN_POINT('Ctrl Pts',(-0.35416671187353,-0.290879136862659,
1.06688848765783));
#3277=CARTESIAN_POINT('Ctrl Pts',(-0.3787731215897,-0.279889827963178,1.05829506364875));
#3278=CARTESIAN_POINT('Ctrl Pts',(-0.425554672694338,-0.251265615809407,
1.04048957871266));
#3279=CARTESIAN_POINT('Ctrl Pts',(-0.452808978448581,-0.227269801620063,
1.02876878445619));
#3280=CARTESIAN_POINT('Ctrl Pts',(-0.493462957200432,-0.177024326825049,
1.0099536580922));
#3281=CARTESIAN_POINT('Ctrl Pts',(-0.511762781179148,-0.14429930310074,
1.00061845128527));
#3282=CARTESIAN_POINT('Ctrl Pts',(-0.529268075276157,-0.0928409665394226,
0.991396466802468));
#3283=CARTESIAN_POINT('Ctrl Pts',(-0.533501897135713,-0.0762225747374254,
0.989110885965947));
#3284=CARTESIAN_POINT('Ctrl Pts',(-0.536443649899848,-0.0595300000000001,
0.987512846410683));
#3285=CARTESIAN_POINT('',(-0.843383895613249,-0.05953,0.742736168477219));
#3286=CARTESIAN_POINT('Origin',(0.,-0.05953,0.));
#3287=CARTESIAN_POINT('',(-1.10653577764992,-0.05953,0.196295654879792));
#3288=CARTESIAN_POINT('Ctrl Pts',(-0.843383895613249,-0.0595300000000001,
0.742736168477219));
#3289=CARTESIAN_POINT('Ctrl Pts',(-0.84559647055299,-0.0762225747374255,
0.740223768851062));
#3290=CARTESIAN_POINT('Ctrl Pts',(-0.848766861100456,-0.0928409665394227,
0.736604687327351));
#3291=CARTESIAN_POINT('Ctrl Pts',(-0.861652925570091,-0.144299303100741,
0.721590372101268));
#3292=CARTESIAN_POINT('Ctrl Pts',(-0.87482617317514,-0.177024326825049,
0.705826641853758));
#3293=CARTESIAN_POINT('Ctrl Pts',(-0.902215926359523,-0.227269801620063,
0.670378702718353));
#3294=CARTESIAN_POINT('Ctrl Pts',(-0.919707509403859,-0.251265615809407,
0.646415841396062));
#3295=CARTESIAN_POINT('Ctrl Pts',(-0.947476448101718,-0.279889827963178,
0.604769294586516));
#3296=CARTESIAN_POINT('Ctrl Pts',(-0.961329858300736,-0.290879136862659,
0.582692035672022));
#3297=CARTESIAN_POINT('Ctrl Pts',(-0.988250837578047,-0.305251990234488,
0.535766169015486));
#3298=CARTESIAN_POINT('Ctrl Pts',(-1.00129756308006,-0.308638795020976,
0.510906605094603));
#3299=CARTESIAN_POINT('Ctrl Pts',(-1.02374168767024,-0.308638795020976,
0.46430090015576));
#3300=CARTESIAN_POINT('Ctrl Pts',(-1.03504317708586,-0.305251990234488,
0.438600874831839));
#3301=CARTESIAN_POINT('Ctrl Pts',(-1.05494634094458,-0.290879136862659,
0.388295406390235));
#3302=CARTESIAN_POINT('Ctrl Pts',(-1.06356957703048,-0.279889827963178,
0.363699428370917));
#3303=CARTESIAN_POINT('Ctrl Pts',(-1.0788165083757,-0.251265615809407,0.316022600643821));
#3304=CARTESIAN_POINT('Ctrl Pts',(-1.08664560412098,-0.227269801620063,
0.287406530683752));
#3305=CARTESIAN_POINT('Ctrl Pts',(-1.09728268713976,-0.177024326825049,
0.243890930799337));
#3306=CARTESIAN_POINT('Ctrl Pts',(-1.10139388218929,-0.144299303100741,
0.22376314604679));
#3307=CARTESIAN_POINT('Ctrl Pts',(-1.10509821673782,-0.0928409665394227,
0.204327142733961));
#3308=CARTESIAN_POINT('Ctrl Pts',(-1.10595102243643,-0.0762225747374254,
0.199591971170104));
#3309=CARTESIAN_POINT('Ctrl Pts',(-1.10653577764992,-0.0595300000000001,
0.196295654879792));
#3310=CARTESIAN_POINT('',(-1.123812,-0.05953,1.37627276864339E-16));
#3311=CARTESIAN_POINT('Origin',(0.,-0.05953,0.));
#3312=CARTESIAN_POINT('',(-1.123812,-0.35718,1.37627276864339E-16));
#3313=CARTESIAN_POINT('',(-1.123812,-0.208355,1.37627276864339E-16));
#3314=CARTESIAN_POINT('Origin',(0.,-0.35718,0.));
#3315=CARTESIAN_POINT('',(-1.10653577764992,-0.05953,-0.196295654879793));
#3316=CARTESIAN_POINT('Origin',(0.,-0.05953,0.));
#3317=CARTESIAN_POINT('',(-0.843383895613249,-0.05953,-0.742736168477219));
#3318=CARTESIAN_POINT('Ctrl Pts',(-1.10653577764992,-0.0595300000000001,
-0.196295654879792));
#3319=CARTESIAN_POINT('Ctrl Pts',(-1.10595102243643,-0.0762225747374255,
-0.199591971170104));
#3320=CARTESIAN_POINT('Ctrl Pts',(-1.10509821673782,-0.0928409665394228,
-0.204327142733962));
#3321=CARTESIAN_POINT('Ctrl Pts',(-1.10139388218929,-0.144299303100741,
-0.22376314604679));
#3322=CARTESIAN_POINT('Ctrl Pts',(-1.09728268713976,-0.177024326825049,
-0.243890930799338));
#3323=CARTESIAN_POINT('Ctrl Pts',(-1.08664560412098,-0.227269801620063,
-0.287406530683753));
#3324=CARTESIAN_POINT('Ctrl Pts',(-1.0788165083757,-0.251265615809407,-0.316022600643821));
#3325=CARTESIAN_POINT('Ctrl Pts',(-1.06356957703048,-0.279889827963178,
-0.363699428370918));
#3326=CARTESIAN_POINT('Ctrl Pts',(-1.05494634094458,-0.290879136862659,
-0.388295406390235));
#3327=CARTESIAN_POINT('Ctrl Pts',(-1.03504317708586,-0.305251990234488,
-0.438600874831839));
#3328=CARTESIAN_POINT('Ctrl Pts',(-1.02374168767024,-0.308638795020976,
-0.46430090015576));
#3329=CARTESIAN_POINT('Ctrl Pts',(-1.00129756308006,-0.308638795020976,
-0.510906605094603));
#3330=CARTESIAN_POINT('Ctrl Pts',(-0.988250837578047,-0.305251990234488,
-0.535766169015486));
#3331=CARTESIAN_POINT('Ctrl Pts',(-0.961329858300736,-0.290879136862659,
-0.582692035672022));
#3332=CARTESIAN_POINT('Ctrl Pts',(-0.947476448101718,-0.279889827963178,
-0.604769294586516));
#3333=CARTESIAN_POINT('Ctrl Pts',(-0.919707509403859,-0.251265615809407,
-0.646415841396062));
#3334=CARTESIAN_POINT('Ctrl Pts',(-0.902215926359523,-0.227269801620064,
-0.670378702718353));
#3335=CARTESIAN_POINT('Ctrl Pts',(-0.87482617317514,-0.177024326825049,
-0.705826641853758));
#3336=CARTESIAN_POINT('Ctrl Pts',(-0.861652925570091,-0.144299303100741,
-0.721590372101268));
#3337=CARTESIAN_POINT('Ctrl Pts',(-0.848766861100456,-0.0928409665394229,
-0.736604687327351));
#3338=CARTESIAN_POINT('Ctrl Pts',(-0.84559647055299,-0.0762225747374255,
-0.740223768851063));
#3339=CARTESIAN_POINT('Ctrl Pts',(-0.843383895613249,-0.0595300000000001,
-0.742736168477219));
#3340=CARTESIAN_POINT('',(-0.536443649899847,-0.05953,-0.987512846410683));
#3341=CARTESIAN_POINT('Origin',(0.,-0.05953,0.));
#3342=CARTESIAN_POINT('',(0.0548532617164172,-0.05953,-1.12247250791415));
#3343=CARTESIAN_POINT('Ctrl Pts',(-0.536443649899848,-0.0595300000000001,
-0.987512846410683));
#3344=CARTESIAN_POINT('Ctrl Pts',(-0.533501897135712,-0.0762225747374254,
-0.989110885965947));
#3345=CARTESIAN_POINT('Ctrl Pts',(-0.529268075276156,-0.0928409665394227,
-0.991396466802469));
#3346=CARTESIAN_POINT('Ctrl Pts',(-0.511762781179147,-0.144299303100741,
-1.00061845128527));
#3347=CARTESIAN_POINT('Ctrl Pts',(-0.493462957200432,-0.177024326825049,
-1.0099536580922));
#3348=CARTESIAN_POINT('Ctrl Pts',(-0.45280897844858,-0.227269801620063,
-1.02876878445619));
#3349=CARTESIAN_POINT('Ctrl Pts',(-0.425554672694337,-0.251265615809407,
-1.04048957871266));
#3350=CARTESIAN_POINT('Ctrl Pts',(-0.3787731215897,-0.279889827963178,-1.05829506364875));
#3351=CARTESIAN_POINT('Ctrl Pts',(-0.354166711873529,-0.290879136862659,
-1.06688848765783));
#3352=CARTESIAN_POINT('Ctrl Pts',(-0.302426893214944,-0.305251990234488,
-1.08269251410343));
#3353=CARTESIAN_POINT('Ctrl Pts',(-0.275287440920027,-0.308638795020976,
-1.0898803575765));
#3354=CARTESIAN_POINT('Ctrl Pts',(-0.224855950742601,-0.308638795020976,
-1.10139101611326));
#3355=CARTESIAN_POINT('Ctrl Pts',(-0.19728546073067,-0.305251990234488,
-1.10669035995599));
#3356=CARTESIAN_POINT('Ctrl Pts',(-0.143812384801039,-0.290879136862659,
-1.11490049012186));
#3357=CARTESIAN_POINT('Ctrl Pts',(-0.117914228755037,-0.279889827963178,
-1.1178344036749));
#3358=CARTESIAN_POINT('Ctrl Pts',(-0.0680399972366989,-0.251265615809407,
-1.12208997038458));
#3359=CARTESIAN_POINT('Ctrl Pts',(-0.0383992541984084,-0.227269801620063,
-1.12335509974011));
#3360=CARTESIAN_POINT('Ctrl Pts',(0.00639229239215326,-0.177024326825049,
-1.12404235695137));
#3361=CARTESIAN_POINT('Ctrl Pts',(0.0269302585198977,-0.144299303100741,
-1.12357162229597));
#3362=CARTESIAN_POINT('Ctrl Pts',(0.04670325263426,-0.0928409665394228,
-1.12285816383385));
#3363=CARTESIAN_POINT('Ctrl Pts',(0.0515094706813703,-0.0762225747374255,
-1.12263591311425));
#3364=CARTESIAN_POINT('Ctrl Pts',(0.0548532617164176,-0.0595300000000001,
-1.12247250791414));
#3365=CARTESIAN_POINT('',(0.437601487681057,-0.05953,-1.03511272300331));
#3366=CARTESIAN_POINT('Origin',(0.,-0.05953,0.));
#3367=CARTESIAN_POINT('',(0.911784794170997,-0.05953,-0.656964154625313));
#3368=CARTESIAN_POINT('Ctrl Pts',(0.437601487681056,-0.0595300000000001,
-1.03511272300331));
#3369=CARTESIAN_POINT('Ctrl Pts',(0.440685038163619,-0.0762225747374255,
-1.03380912944435));
#3370=CARTESIAN_POINT('Ctrl Pts',(0.445111721969657,-0.0928409665394228,
-1.03192403056628));
#3371=CARTESIAN_POINT('Ctrl Pts',(0.463236132117164,-0.144299303100741,
-1.0239876538093));
#3372=CARTESIAN_POINT('Ctrl Pts',(0.481944444320713,-0.177024326825049,
-1.01550068154148));
#3373=CARTESIAN_POINT('Ctrl Pts',(0.522002043615455,-0.227269801620064,
-0.995447160474328));
#3374=CARTESIAN_POINT('Ctrl Pts',(0.548158511259203,-0.251265615809407,
-0.981446681891443));
#3375=CARTESIAN_POINT('Ctrl Pts',(0.591247219971725,-0.279889827963178,
-0.955972930713954));
#3376=CARTESIAN_POINT('Ctrl Pts',(0.613307674922609,-0.290879136862659,
-0.942092777160053));
#3377=CARTESIAN_POINT('Ctrl Pts',(0.657923009631182,-0.305251990234487,
-0.91149460735272));
#3378=CARTESIAN_POINT('Ctrl Pts',(0.680463863683393,-0.308638795020976,
-0.894757676234429));
#3379=CARTESIAN_POINT('Ctrl Pts',(0.720906778729542,-0.308638795020976,
-0.862505527716294));
#3380=CARTESIAN_POINT('Ctrl Pts',(0.742239891936899,-0.305251990234488,
-0.844254137480381));
#3381=CARTESIAN_POINT('Ctrl Pts',(0.781998747691872,-0.290879136862659,
-0.80756613568454));
#3382=CARTESIAN_POINT('Ctrl Pts',(0.800439809856112,-0.279889827963178,
-0.789147407129765));
#3383=CARTESIAN_POINT('Ctrl Pts',(0.834863020612702,-0.251265615809407,
-0.752807465209441));
#3384=CARTESIAN_POINT('Ctrl Pts',(0.854332839576145,-0.227269801620064,
-0.73042219438957));
#3385=CARTESIAN_POINT('Ctrl Pts',(0.882797231409153,-0.177024326825049,
-0.695831250979106));
#3386=CARTESIAN_POINT('Ctrl Pts',(0.895234408667242,-0.144299303100741,
-0.679480524217551));
#3387=CARTESIAN_POINT('Ctrl Pts',(0.907004864562642,-0.0928409665394228,
-0.663576540841106));
#3388=CARTESIAN_POINT('Ctrl Pts',(0.909827729890942,-0.0762225747374256,
-0.659680317203144));
#3389=CARTESIAN_POINT('Ctrl Pts',(0.911784794170998,-0.0595300000000001,
-0.656964154625312));
#3390=CARTESIAN_POINT('',(1.08212377959455,-0.05953,-0.303251606722892));
#3391=CARTESIAN_POINT('Origin',(0.,-0.05953,0.));
#3392=CARTESIAN_POINT('',(1.08212377959455,-0.05953,0.303251606722892));
#3393=CARTESIAN_POINT('Ctrl Pts',(1.08212377959455,-0.0595300000000001,
-0.303251606722892));
#3394=CARTESIAN_POINT('Ctrl Pts',(1.0830271513892,-0.0762225747374255,-0.300028012588062));
#3395=CARTESIAN_POINT('Ctrl Pts',(1.08431331394788,-0.0928409665394228,
-0.2953917518996));
#3396=CARTESIAN_POINT('Ctrl Pts',(1.08940878963422,-0.144299303100741,-0.276273267473431));
#3397=CARTESIAN_POINT('Ctrl Pts',(1.09443784939331,-0.177024326825049,-0.256354979351213));
#3398=CARTESIAN_POINT('Ctrl Pts',(1.10373487993589,-0.227269801620064,-0.212533521233765));
#3399=CARTESIAN_POINT('Ctrl Pts',(1.10909715583869,-0.251265615809407,-0.183354415742157));
#3400=CARTESIAN_POINT('Ctrl Pts',(1.1160463456491,-0.279889827963178,-0.133783682657561));
#3401=CARTESIAN_POINT('Ctrl Pts',(1.11894887330541,-0.290879136862659,-0.107881990270302));
#3402=CARTESIAN_POINT('Ctrl Pts',(1.12284346704144,-0.305251990234488,-0.0539226701638766));
#3403=CARTESIAN_POINT('Ctrl Pts',(1.123812,-0.308638795020976,-0.025864214957475));
#3404=CARTESIAN_POINT('Ctrl Pts',(1.123812,-0.308638795020976,0.025864214957475));
#3405=CARTESIAN_POINT('Ctrl Pts',(1.12284346704144,-0.305251990234488,0.0539226701638766));
#3406=CARTESIAN_POINT('Ctrl Pts',(1.11894887330541,-0.290879136862659,0.107881990270302));
#3407=CARTESIAN_POINT('Ctrl Pts',(1.1160463456491,-0.279889827963178,0.133783682657561));
#3408=CARTESIAN_POINT('Ctrl Pts',(1.10909715583869,-0.251265615809407,0.183354415742157));
#3409=CARTESIAN_POINT('Ctrl Pts',(1.10373487993589,-0.227269801620064,0.212533521233765));
#3410=CARTESIAN_POINT('Ctrl Pts',(1.09443784939331,-0.177024326825049,0.256354979351213));
#3411=CARTESIAN_POINT('Ctrl Pts',(1.08940878963422,-0.144299303100741,0.276273267473431));
#3412=CARTESIAN_POINT('Ctrl Pts',(1.08431331394788,-0.0928409665394228,
0.2953917518996));
#3413=CARTESIAN_POINT('Ctrl Pts',(1.0830271513892,-0.0762225747374255,0.300028012588062));
#3414=CARTESIAN_POINT('Ctrl Pts',(1.08212377959455,-0.0595300000000001,
0.303251606722892));
#3415=CARTESIAN_POINT('Origin',(0.,-0.05953,0.));
#3416=CARTESIAN_POINT('Origin',(0.,-0.05953,0.));
#3417=CARTESIAN_POINT('',(0.0589974094846122,-0.05953,1.07456964270265));
#3418=CARTESIAN_POINT('Origin',(0.,-0.05953,0.));
#3419=CARTESIAN_POINT('Origin',(-0.244773027351946,-0.05953,1.07242070340001));
#3420=CARTESIAN_POINT('Origin',(-0.244773027351946,0.,1.07242070340001));
#3421=CARTESIAN_POINT('',(-0.519393123750572,-0.05953,0.942555777842682));
#3422=CARTESIAN_POINT('Ctrl Pts',(-0.519393123750572,-0.05953,0.942555777842682));
#3423=CARTESIAN_POINT('Ctrl Pts',(-0.513714466572041,-0.0925528133349865,
0.945684988399766));
#3424=CARTESIAN_POINT('Ctrl Pts',(-0.503136848051455,-0.124911173756694,
0.951483858396181));
#3425=CARTESIAN_POINT('Ctrl Pts',(-0.47593627990192,-0.177924977804098,
0.965323333309091));
#3426=CARTESIAN_POINT('Ctrl Pts',(-0.460931856495794,-0.199697230012983,
0.972669835243841));
#3427=CARTESIAN_POINT('Ctrl Pts',(-0.426157505475872,-0.237895043532788,
0.988400002689705));
#3428=CARTESIAN_POINT('Ctrl Pts',(-0.406380688682952,-0.254319232363049,
0.996771768218699));
#3429=CARTESIAN_POINT('Ctrl Pts',(-0.364750145543744,-0.28018331644634,
1.01272583306292));
#3430=CARTESIAN_POINT('Ctrl Pts',(-0.340838910881557,-0.29104845371857,
1.02112815447116));
#3431=CARTESIAN_POINT('Ctrl Pts',(-0.290495481564827,-0.30527573347708,
1.036574285215));
#3432=CARTESIAN_POINT('Ctrl Pts',(-0.264056468041074,-0.308638795020976,
1.04359501395068));
#3433=CARTESIAN_POINT('Ctrl Pts',(-0.214892249704082,-0.308638795020976,
1.05481642595959));
#3434=CARTESIAN_POINT('Ctrl Pts',(-0.188025341585962,-0.30527573347708,
1.05996242598502));
#3435=CARTESIAN_POINT('Ctrl Pts',(-0.135965654106109,-0.29104845371857,
1.06788913840721));
#3436=CARTESIAN_POINT('Ctrl Pts',(-0.110776745452494,-0.28018331644634,
1.07069360430242));
#3437=CARTESIAN_POINT('Ctrl Pts',(-0.0663467128214646,-0.254319232363049,
1.07438230428002));
#3438=CARTESIAN_POINT('Ctrl Pts',(-0.0448960436540983,-0.237895043532788,
1.07542044338697));
#3439=CARTESIAN_POINT('Ctrl Pts',(-0.00674037211528124,-0.199697230012983,
1.07633607767727));
#3440=CARTESIAN_POINT('Ctrl Pts',(0.00996567398334777,-0.177924977804098,
1.07622728347683));
#3441=CARTESIAN_POINT('Ctrl Pts',(0.0404772621979741,-0.124911173756694,
1.07556023164702));
#3442=CARTESIAN_POINT('Ctrl Pts',(0.0525234025782719,-0.0925528133349865,
1.07492508698591));
#3443=CARTESIAN_POINT('Ctrl Pts',(0.0589974094846124,-0.05953,1.07456964270265));
#3444=CARTESIAN_POINT('Origin',(-0.244773027351946,-0.05953,1.07242070340001));
#3445=CARTESIAN_POINT('Origin',(0.,-0.05953,0.));
#3446=CARTESIAN_POINT('',(-0.803348093619616,-0.05953,0.716109245731214));
#3447=CARTESIAN_POINT('Origin',(0.,-0.05953,0.));
#3448=CARTESIAN_POINT('Origin',(-0.991065754692661,-0.05953,0.477272113029314));
#3449=CARTESIAN_POINT('Origin',(-0.991065754692661,0.,0.477272113029314));
#3450=CARTESIAN_POINT('',(-1.06075609691358,-0.05953,0.181596019242328));
#3451=CARTESIAN_POINT('Ctrl Pts',(-1.06075609691358,-0.05953,0.181596019242328));
#3452=CARTESIAN_POINT('Ctrl Pts',(-1.05966202740332,-0.0925528133349865,
0.187986803072856));
#3453=CARTESIAN_POINT('Ctrl Pts',(-1.05760072925372,-0.124911173756694,
0.199872254546857));
#3454=CARTESIAN_POINT('Ctrl Pts',(-1.05146158959546,-0.177924977804098,
0.22976728653846));
#3455=CARTESIAN_POINT('Ctrl Pts',(-1.04785021111757,-0.199697230012983,
0.246078686169301));
#3456=CARTESIAN_POINT('Ctrl Pts',(-1.03846709802406,-0.237895043532788,
0.283073967563097));
#3457=CARTESIAN_POINT('Ctrl Pts',(-1.03268176429485,-0.254319232363049,
0.303755815985685));
#3458=CARTESIAN_POINT('Ctrl Pts',(-1.01919893537026,-0.28018331644634,0.346251081972725));
#3459=CARTESIAN_POINT('Ctrl Pts',(-1.01085972381132,-0.29104845371857,0.370184399726282));
#3460=CARTESIAN_POINT('Ctrl Pts',(-0.99154738033959,-0.30527573347708,0.419174982698463));
#3461=CARTESIAN_POINT('Ctrl Pts',(-0.980551951791748,-0.308638795020976,
0.444223188605045));
#3462=CARTESIAN_POINT('Ctrl Pts',(-0.958671816228589,-0.308638795020976,
0.489657758261848));
#3463=CARTESIAN_POINT('Ctrl Pts',(-0.945943877838127,-0.30527573347708,
0.51387163140139));
#3464=CARTESIAN_POINT('Ctrl Pts',(-0.91968254693063,-0.29104845371857,0.559515758398093));
#3465=CARTESIAN_POINT('Ctrl Pts',(-0.906170138993533,-0.28018331644634,
0.580957796077825));
#3466=CARTESIAN_POINT('Ctrl Pts',(-0.8813524085237,-0.254319232363049,0.617994461173994));
#3467=CARTESIAN_POINT('Ctrl Pts',(-0.868789784891799,-0.237895043532788,
0.635412538795143));
#3468=CARTESIAN_POINT('Ctrl Pts',(-0.845715984518854,-0.199697230012983,
0.66581473268113));
#3469=CARTESIAN_POINT('Ctrl Pts',(-0.835214876415962,-0.177924977804098,
0.678808213394124));
#3470=CARTESIAN_POINT('Ctrl Pts',(-0.815669690204649,-0.124911173756694,
0.702247233627224));
#3471=CARTESIAN_POINT('Ctrl Pts',(-0.807662468433796,-0.0925528133349865,
0.711269279199861));
#3472=CARTESIAN_POINT('Ctrl Pts',(-0.803348093619616,-0.05953,0.716109245731214));
#3473=CARTESIAN_POINT('Origin',(-0.991065754692661,-0.05953,0.477272113029314));
#3474=CARTESIAN_POINT('Origin',(0.,-0.05953,0.));
#3475=CARTESIAN_POINT('',(-1.076188,-0.05953,1.31795018948079E-16));
#3476=CARTESIAN_POINT('Origin',(0.,-0.05953,0.));
#3477=CARTESIAN_POINT('',(-1.06075609691358,-0.05953,-0.181596019242328));
#3478=CARTESIAN_POINT('Origin',(0.,-0.05953,0.));
#3479=CARTESIAN_POINT('Origin',(-0.991065754692661,-0.05953,-0.477272113029314));
#3480=CARTESIAN_POINT('Origin',(-0.991065754692661,0.,-0.477272113029314));
#3481=CARTESIAN_POINT('',(-0.803348093619616,-0.05953,-0.716109245731215));
#3482=CARTESIAN_POINT('Ctrl Pts',(-0.803348093619616,-0.05953,-0.716109245731215));
#3483=CARTESIAN_POINT('Ctrl Pts',(-0.807662468433795,-0.0925528133349865,
-0.711269279199862));
#3484=CARTESIAN_POINT('Ctrl Pts',(-0.815669690204649,-0.124911173756694,
-0.702247233627224));
#3485=CARTESIAN_POINT('Ctrl Pts',(-0.835214876415962,-0.177924977804098,
-0.678808213394124));
#3486=CARTESIAN_POINT('Ctrl Pts',(-0.845715984518854,-0.199697230012983,
-0.66581473268113));
#3487=CARTESIAN_POINT('Ctrl Pts',(-0.868789784891799,-0.237895043532788,
-0.635412538795143));
#3488=CARTESIAN_POINT('Ctrl Pts',(-0.8813524085237,-0.254319232363049,-0.617994461173994));
#3489=CARTESIAN_POINT('Ctrl Pts',(-0.906170138993533,-0.28018331644634,
-0.580957796077826));
#3490=CARTESIAN_POINT('Ctrl Pts',(-0.91968254693063,-0.29104845371857,-0.559515758398093));
#3491=CARTESIAN_POINT('Ctrl Pts',(-0.945943877838127,-0.30527573347708,
-0.51387163140139));
#3492=CARTESIAN_POINT('Ctrl Pts',(-0.958671816228589,-0.308638795020976,
-0.489657758261848));
#3493=CARTESIAN_POINT('Ctrl Pts',(-0.980551951791748,-0.308638795020976,
-0.444223188605045));
#3494=CARTESIAN_POINT('Ctrl Pts',(-0.99154738033959,-0.30527573347708,-0.419174982698463));
#3495=CARTESIAN_POINT('Ctrl Pts',(-1.01085972381132,-0.29104845371857,-0.370184399726282));
#3496=CARTESIAN_POINT('Ctrl Pts',(-1.01919893537026,-0.28018331644634,-0.346251081972725));
#3497=CARTESIAN_POINT('Ctrl Pts',(-1.03268176429485,-0.254319232363049,
-0.303755815985685));
#3498=CARTESIAN_POINT('Ctrl Pts',(-1.03846709802406,-0.237895043532788,
-0.283073967563097));
#3499=CARTESIAN_POINT('Ctrl Pts',(-1.04785021111757,-0.199697230012983,
-0.246078686169302));
#3500=CARTESIAN_POINT('Ctrl Pts',(-1.05146158959546,-0.177924977804098,
-0.229767286538461));
#3501=CARTESIAN_POINT('Ctrl Pts',(-1.05760072925372,-0.124911173756694,
-0.199872254546858));
#3502=CARTESIAN_POINT('Ctrl Pts',(-1.05966202740332,-0.0925528133349864,
-0.187986803072857));
#3503=CARTESIAN_POINT('Ctrl Pts',(-1.06075609691358,-0.05953,-0.181596019242328));
#3504=CARTESIAN_POINT('Origin',(-0.991065754692661,-0.05953,-0.477272113029314));
#3505=CARTESIAN_POINT('Origin',(0.,-0.05953,0.));
#3506=CARTESIAN_POINT('',(-0.519393123750572,-0.05953,-0.942555777842682));
#3507=CARTESIAN_POINT('Origin',(0.,-0.05953,0.));
#3508=CARTESIAN_POINT('Origin',(-0.244773027351946,-0.05953,-1.07242070340001));
#3509=CARTESIAN_POINT('Origin',(-0.244773027351946,0.,-1.07242070340001));
#3510=CARTESIAN_POINT('',(0.0589974094846125,-0.05953,-1.07456964270265));
#3511=CARTESIAN_POINT('Ctrl Pts',(0.0589974094846127,-0.05953,-1.07456964270265));
#3512=CARTESIAN_POINT('Ctrl Pts',(0.0525234025782722,-0.0925528133349865,
-1.07492508698591));
#3513=CARTESIAN_POINT('Ctrl Pts',(0.0404772621979744,-0.124911173756694,
-1.07556023164702));
#3514=CARTESIAN_POINT('Ctrl Pts',(0.0099656739833481,-0.177924977804098,
-1.07622728347683));
#3515=CARTESIAN_POINT('Ctrl Pts',(-0.00674037211528096,-0.199697230012983,
-1.07633607767727));
#3516=CARTESIAN_POINT('Ctrl Pts',(-0.044896043654098,-0.237895043532788,
-1.07542044338697));
#3517=CARTESIAN_POINT('Ctrl Pts',(-0.0663467128214644,-0.254319232363049,
-1.07438230428002));
#3518=CARTESIAN_POINT('Ctrl Pts',(-0.110776745452493,-0.28018331644634,
-1.07069360430242));
#3519=CARTESIAN_POINT('Ctrl Pts',(-0.135965654106109,-0.29104845371857,
-1.06788913840721));
#3520=CARTESIAN_POINT('Ctrl Pts',(-0.188025341585962,-0.30527573347708,
-1.05996242598502));
#3521=CARTESIAN_POINT('Ctrl Pts',(-0.214892249704082,-0.308638795020976,
-1.05481642595959));
#3522=CARTESIAN_POINT('Ctrl Pts',(-0.264056468041074,-0.308638795020976,
-1.04359501395068));
#3523=CARTESIAN_POINT('Ctrl Pts',(-0.290495481564827,-0.30527573347708,
-1.036574285215));
#3524=CARTESIAN_POINT('Ctrl Pts',(-0.340838910881557,-0.291048453718569,
-1.02112815447116));
#3525=CARTESIAN_POINT('Ctrl Pts',(-0.364750145543744,-0.28018331644634,
-1.01272583306292));
#3526=CARTESIAN_POINT('Ctrl Pts',(-0.406380688682952,-0.254319232363049,
-0.996771768218699));
#3527=CARTESIAN_POINT('Ctrl Pts',(-0.426157505475872,-0.237895043532788,
-0.988400002689705));
#3528=CARTESIAN_POINT('Ctrl Pts',(-0.460931856495794,-0.199697230012983,
-0.972669835243841));
#3529=CARTESIAN_POINT('Ctrl Pts',(-0.475936279901919,-0.177924977804098,
-0.965323333309091));
#3530=CARTESIAN_POINT('Ctrl Pts',(-0.503136848051454,-0.124911173756694,
-0.951483858396181));
#3531=CARTESIAN_POINT('Ctrl Pts',(-0.513714466572041,-0.0925528133349865,
-0.945684988399766));
#3532=CARTESIAN_POINT('Ctrl Pts',(-0.519393123750572,-0.05953,-0.942555777842682));
#3533=CARTESIAN_POINT('Origin',(-0.244773027351946,-0.05953,-1.07242070340001));
#3534=CARTESIAN_POINT('Origin',(0.,-0.05953,0.));
#3535=CARTESIAN_POINT('',(0.413083465285518,-0.05953,-0.993751811093549));
#3536=CARTESIAN_POINT('Origin',(0.,-0.05953,0.));
#3537=CARTESIAN_POINT('Origin',(0.685838782044607,-0.05953,-0.860014630714833));
#3538=CARTESIAN_POINT('Origin',(0.685838782044607,0.,-0.860014630714833));
#3539=CARTESIAN_POINT('',(0.876916659919095,-0.05953,-0.623857181492959));
#3540=CARTESIAN_POINT('Ctrl Pts',(0.876916659919095,-0.05953,-0.623857181492958));
#3541=CARTESIAN_POINT('Ctrl Pts',(0.873158080166742,-0.0925528133349865,
-0.62914037979579));
#3542=CARTESIAN_POINT('Ctrl Pts',(0.866144010579847,-0.124911173756694,
-0.638954437806245));
#3543=CARTESIAN_POINT('Ctrl Pts',(0.847641868610495,-0.177924977804098,
-0.663225258065736));
#3544=CARTESIAN_POINT('Ctrl Pts',(0.837310877969633,-0.199697230012983,
-0.676354402927683));
#3545=CARTESIAN_POINT('Ctrl Pts',(0.81280533416753,-0.237895043532788,-0.705614819529209));
#3546=CARTESIAN_POINT('Ctrl Pts',(0.798619410861634,-0.254319232363049,
-0.721738358858166));
#3547=CARTESIAN_POINT('Ctrl Pts',(0.768033796848072,-0.28018331644634,-0.754175290318038));
#3548=CARTESIAN_POINT('Ctrl Pts',(0.750136149454208,-0.29104845371857,-0.772120216227122));
#3549=CARTESIAN_POINT('Ctrl Pts',(0.711480111898423,-0.30527573347708,-0.807879894508811));
#3550=CARTESIAN_POINT('Ctrl Pts',(0.690705563850638,-0.308638795020976,
-0.825676810575913));
#3551=CARTESIAN_POINT('Ctrl Pts',(0.651278921914856,-0.308638795020976,
-0.857118508332695));
#3552=CARTESIAN_POINT('Ctrl Pts',(0.629305439856167,-0.30527573347708,-0.873412008702649));
#3553=CARTESIAN_POINT('Ctrl Pts',(0.585840553788742,-0.29104845371857,-0.903141581680914));
#3554=CARTESIAN_POINT('Ctrl Pts',(0.564362943424239,-0.28018331644634,-0.916597376014514));
#3555=CARTESIAN_POINT('Ctrl Pts',(0.525933334162556,-0.254319232363049,
-0.939198248544427));
#3556=CARTESIAN_POINT('Ctrl Pts',(0.507057380724533,-0.237895043532788,
-0.949440676105255));
#3557=CARTESIAN_POINT('Ctrl Pts',(0.473077587363686,-0.199697230012983,
-0.966820759530997));
#3558=CARTESIAN_POINT('Ctrl Pts',(0.457978755888596,-0.177924977804098,
-0.973971221090534));
#3559=CARTESIAN_POINT('Ctrl Pts',(0.430199341854858,-0.124911173756694,
-0.986608710139579));
#3560=CARTESIAN_POINT('Ctrl Pts',(0.419070565453384,-0.0925528133349865,
-0.991263089003441));
#3561=CARTESIAN_POINT('Ctrl Pts',(0.413083465285518,-0.05953,-0.993751811093549));
#3562=CARTESIAN_POINT('Origin',(0.685838782044607,-0.05953,-0.860014630714833));
#3563=CARTESIAN_POINT('Origin',(0.,-0.208355,0.));
#3564=CARTESIAN_POINT('',(-1.076188,-0.35718,1.31795018948079E-16));
#3565=CARTESIAN_POINT('Origin',(0.,-0.35718,0.));
#3566=CARTESIAN_POINT('',(-1.076188,-0.208355,1.31795018948079E-16));
#3567=CARTESIAN_POINT('',(1.03449977959455,-0.05953,0.296632461748266));
#3568=CARTESIAN_POINT('Origin',(0.,-0.05953,0.));
#3569=CARTESIAN_POINT('',(1.03449977959455,-0.05953,-0.296632461748266));
#3570=CARTESIAN_POINT('Ctrl Pts',(1.03449977959455,-0.05953,0.296632461748267));
#3571=CARTESIAN_POINT('Ctrl Pts',(1.03628691421076,-0.0925528133349865,
0.290399865505497));
#3572=CARTESIAN_POINT('Ctrl Pts',(1.03958665287714,-0.124911173756694,0.278797079997872));
#3573=CARTESIAN_POINT('Ctrl Pts',(1.0470264474309,-0.177924977804098,0.249198913998601));
#3574=CARTESIAN_POINT('Ctrl Pts',(1.05084995891418,-0.199697230012983,0.232935932341942));
#3575=CARTESIAN_POINT('Ctrl Pts',(1.05844771715377,-0.237895043532788,0.195533155353269));
#3576=CARTESIAN_POINT('Ctrl Pts',(1.06220882929878,-0.254319232363049,0.17438929156337));
#3577=CARTESIAN_POINT('Ctrl Pts',(1.06849922508772,-0.28018331644634,0.130252399648131));
#3578=CARTESIAN_POINT('Ctrl Pts',(1.07137013248666,-0.29104845371857,0.105070977154072));
#3579=CARTESIAN_POINT('Ctrl Pts',(1.07522652957392,-0.30527573347708,0.0525526752791107));
#3580=CARTESIAN_POINT('Ctrl Pts',(1.076188,-0.308638795020976,0.025214283908933));
#3581=CARTESIAN_POINT('Ctrl Pts',(1.076188,-0.308638795020976,-0.025214283908933));
#3582=CARTESIAN_POINT('Ctrl Pts',(1.07522652957392,-0.30527573347708,-0.0525526752791107));
#3583=CARTESIAN_POINT('Ctrl Pts',(1.07137013248666,-0.29104845371857,-0.105070977154072));
#3584=CARTESIAN_POINT('Ctrl Pts',(1.06849922508772,-0.28018331644634,-0.130252399648131));
#3585=CARTESIAN_POINT('Ctrl Pts',(1.06220882929878,-0.254319232363049,-0.17438929156337));
#3586=CARTESIAN_POINT('Ctrl Pts',(1.05844771715377,-0.237895043532788,-0.195533155353269));
#3587=CARTESIAN_POINT('Ctrl Pts',(1.05084995891418,-0.199697230012983,-0.232935932341942));
#3588=CARTESIAN_POINT('Ctrl Pts',(1.0470264474309,-0.177924977804098,-0.249198913998601));
#3589=CARTESIAN_POINT('Ctrl Pts',(1.03958665287714,-0.124911173756694,-0.278797079997872));
#3590=CARTESIAN_POINT('Ctrl Pts',(1.03628691421076,-0.0925528133349865,
-0.290399865505497));
#3591=CARTESIAN_POINT('Ctrl Pts',(1.03449977959455,-0.05953,-0.296632461748267));
#3592=CARTESIAN_POINT('Origin',(0.,-0.05953,0.));
#3593=CARTESIAN_POINT('Origin',(0.,-0.05953,0.));
#3594=CARTESIAN_POINT('Origin',(1.1,-0.05953,0.));
#3595=CARTESIAN_POINT('Origin',(1.1,0.,0.));
#3596=CARTESIAN_POINT('Origin',(1.1,-0.05953,0.));
#3597=CARTESIAN_POINT('Origin',(0.,-0.35718,0.));
#3598=CARTESIAN_POINT('Origin',(0.,-0.05953,0.));
#3599=CARTESIAN_POINT('',(0.,0.,0.));
#3600=CARTESIAN_POINT('Origin',(1.119765,0.495,0.));
#3601=CARTESIAN_POINT('',(-1.119765,0.495,-1.37131662304724E-16));
#3602=CARTESIAN_POINT('Origin',(0.,0.495,0.));
#3603=CARTESIAN_POINT('',(-1.085235,0.495,-1.32902956907268E-16));
#3604=CARTESIAN_POINT('Origin',(0.,0.495,0.));
#3605=CARTESIAN_POINT('Origin',(0.,0.4575,0.));
#3606=CARTESIAN_POINT('',(-1.119765,0.42,-1.37131662304724E-16));
#3607=CARTESIAN_POINT('Origin',(0.,0.42,0.));
#3608=CARTESIAN_POINT('',(-1.119765,0.4575,-1.37131662304724E-16));
#3609=CARTESIAN_POINT('Origin',(1.085235,0.42,0.));
#3610=CARTESIAN_POINT('',(-1.085235,0.42,-1.32902956907268E-16));
#3611=CARTESIAN_POINT('Origin',(0.,0.42,0.));
#3612=CARTESIAN_POINT('Origin',(0.,0.4575,0.));
#3613=CARTESIAN_POINT('',(-1.085235,0.4575,-1.32902956907268E-16));
#3614=CARTESIAN_POINT('Origin',(1.119765,-0.42,0.));
#3615=CARTESIAN_POINT('',(-1.119765,-0.42,-1.37131662304724E-16));
#3616=CARTESIAN_POINT('Origin',(0.,-0.42,0.));
#3617=CARTESIAN_POINT('',(-1.085235,-0.42,-1.32902956907268E-16));
#3618=CARTESIAN_POINT('Origin',(0.,-0.42,0.));
#3619=CARTESIAN_POINT('Origin',(0.,-0.4575,0.));
#3620=CARTESIAN_POINT('',(-1.119765,-0.495,-1.37131662304724E-16));
#3621=CARTESIAN_POINT('Origin',(0.,-0.495,0.));
#3622=CARTESIAN_POINT('',(-1.119765,-0.4575,-1.37131662304724E-16));
#3623=CARTESIAN_POINT('Origin',(1.085235,-0.495,0.));
#3624=CARTESIAN_POINT('',(-1.085235,-0.495,-1.32902956907268E-16));
#3625=CARTESIAN_POINT('Origin',(0.,-0.495,0.));
#3626=CARTESIAN_POINT('Origin',(0.,-0.4575,0.));
#3627=CARTESIAN_POINT('',(-1.085235,-0.4575,-1.32902956907268E-16));
#3628=CARTESIAN_POINT('',(0.,0.,0.));
#3629=CARTESIAN_POINT('',(0.,0.,0.));
#3630=CARTESIAN_POINT('',(0.,0.,0.));
#3631=CARTESIAN_POINT('',(0.,0.,0.));
#3632=CARTESIAN_POINT('',(0.,0.,0.));
#3633=CARTESIAN_POINT('',(0.,0.,0.));
#3634=CARTESIAN_POINT('Origin',(0.,1.1,3.5));
#3635=CARTESIAN_POINT('',(-1.2,1.3,3.5));
#3636=CARTESIAN_POINT('Origin',(0.,1.3,3.5));
#3637=CARTESIAN_POINT('',(-1.2,1.1,3.5));
#3638=CARTESIAN_POINT('',(-1.2,1.1,3.5));
#3639=CARTESIAN_POINT('Origin',(0.,1.1,3.5));
#3640=CARTESIAN_POINT('Origin',(0.,1.1,3.5));
#3641=CARTESIAN_POINT('',(-1.6,1.3,3.5));
#3642=CARTESIAN_POINT('Origin',(0.,1.3,3.5));
#3643=CARTESIAN_POINT('',(-1.6,1.1,3.5));
#3644=CARTESIAN_POINT('',(-1.6,1.1,3.5));
#3645=CARTESIAN_POINT('Origin',(0.,1.1,3.5));
#3646=CARTESIAN_POINT('Origin',(0.,1.3,3.5));
#3647=CARTESIAN_POINT('Origin',(0.,1.1,3.5));
#3648=CARTESIAN_POINT('',(0.,0.,0.));
#3649=CARTESIAN_POINT('',(0.,0.,0.));
#3650=CARTESIAN_POINT('',(0.,-0.6,3.5));
#3651=CARTESIAN_POINT('',(0.,0.6,3.5));
#3652=CARTESIAN_POINT('',(0.,-2.4,0.));
#3653=CARTESIAN_POINT('',(0.,0.,0.));
#3654=CARTESIAN_POINT('',(0.,0.,0.));
#3655=UNCERTAINTY_MEASURE_WITH_UNIT(LENGTH_MEASURE(0.001),#3689,
'DISTANCE_ACCURACY_VALUE',
'Maximum model space distance between geometric entities at asserted c
onnectivities');
#3656=UNCERTAINTY_MEASURE_WITH_UNIT(LENGTH_MEASURE(0.001),#3689,
'DISTANCE_ACCURACY_VALUE',
'Maximum model space distance between geometric entities at asserted c
onnectivities');
#3657=UNCERTAINTY_MEASURE_WITH_UNIT(LENGTH_MEASURE(0.001),#3689,
'DISTANCE_ACCURACY_VALUE',
'Maximum model space distance between geometric entities at asserted c
onnectivities');
#3658=UNCERTAINTY_MEASURE_WITH_UNIT(LENGTH_MEASURE(0.001),#3689,
'DISTANCE_ACCURACY_VALUE',
'Maximum model space distance between geometric entities at asserted c
onnectivities');
#3659=UNCERTAINTY_MEASURE_WITH_UNIT(LENGTH_MEASURE(0.001),#3689,
'DISTANCE_ACCURACY_VALUE',
'Maximum model space distance between geometric entities at asserted c
onnectivities');
#3660=UNCERTAINTY_MEASURE_WITH_UNIT(LENGTH_MEASURE(0.001),#3689,
'DISTANCE_ACCURACY_VALUE',
'Maximum model space distance between geometric entities at asserted c
onnectivities');
#3661=UNCERTAINTY_MEASURE_WITH_UNIT(LENGTH_MEASURE(0.001),#3689,
'DISTANCE_ACCURACY_VALUE',
'Maximum model space distance between geometric entities at asserted c
onnectivities');
#3662=UNCERTAINTY_MEASURE_WITH_UNIT(LENGTH_MEASURE(0.001),#3689,
'DISTANCE_ACCURACY_VALUE',
'Maximum model space distance between geometric entities at asserted c
onnectivities');
#3663=UNCERTAINTY_MEASURE_WITH_UNIT(LENGTH_MEASURE(0.001),#3689,
'DISTANCE_ACCURACY_VALUE',
'Maximum model space distance between geometric entities at asserted c
onnectivities');
#3664=UNCERTAINTY_MEASURE_WITH_UNIT(LENGTH_MEASURE(0.001),#3689,
'DISTANCE_ACCURACY_VALUE',
'Maximum model space distance between geometric entities at asserted c
onnectivities');
#3665=UNCERTAINTY_MEASURE_WITH_UNIT(LENGTH_MEASURE(0.001),#3689,
'DISTANCE_ACCURACY_VALUE',
'Maximum model space distance between geometric entities at asserted c
onnectivities');
#3666=UNCERTAINTY_MEASURE_WITH_UNIT(LENGTH_MEASURE(0.001),#3689,
'DISTANCE_ACCURACY_VALUE',
'Maximum model space distance between geometric entities at asserted c
onnectivities');
#3667=UNCERTAINTY_MEASURE_WITH_UNIT(LENGTH_MEASURE(0.001),#3689,
'DISTANCE_ACCURACY_VALUE',
'Maximum model space distance between geometric entities at asserted c
onnectivities');
#3668=UNCERTAINTY_MEASURE_WITH_UNIT(LENGTH_MEASURE(0.001),#3689,
'DISTANCE_ACCURACY_VALUE',
'Maximum model space distance between geometric entities at asserted c
onnectivities');
#3669=UNCERTAINTY_MEASURE_WITH_UNIT(LENGTH_MEASURE(0.001),#3689,
'DISTANCE_ACCURACY_VALUE',
'Maximum model space distance between geometric entities at asserted c
onnectivities');
#3670=UNCERTAINTY_MEASURE_WITH_UNIT(LENGTH_MEASURE(0.001),#3689,
'DISTANCE_ACCURACY_VALUE',
'Maximum model space distance between geometric entities at asserted c
onnectivities');
#3671=UNCERTAINTY_MEASURE_WITH_UNIT(LENGTH_MEASURE(0.001),#3689,
'DISTANCE_ACCURACY_VALUE',
'Maximum model space distance between geometric entities at asserted c
onnectivities');
#3672=(
GEOMETRIC_REPRESENTATION_CONTEXT(3)
GLOBAL_UNCERTAINTY_ASSIGNED_CONTEXT((#3655))
GLOBAL_UNIT_ASSIGNED_CONTEXT((#3689,#3691,#3692))
REPRESENTATION_CONTEXT('','3D')
);
#3673=(
GEOMETRIC_REPRESENTATION_CONTEXT(3)
GLOBAL_UNCERTAINTY_ASSIGNED_CONTEXT((#3656))
GLOBAL_UNIT_ASSIGNED_CONTEXT((#3689,#3691,#3692))
REPRESENTATION_CONTEXT('','3D')
);
#3674=(
GEOMETRIC_REPRESENTATION_CONTEXT(3)
GLOBAL_UNCERTAINTY_ASSIGNED_CONTEXT((#3657))
GLOBAL_UNIT_ASSIGNED_CONTEXT((#3689,#3691,#3692))
REPRESENTATION_CONTEXT('','3D')
);
#3675=(
GEOMETRIC_REPRESENTATION_CONTEXT(3)
GLOBAL_UNCERTAINTY_ASSIGNED_CONTEXT((#3658))
GLOBAL_UNIT_ASSIGNED_CONTEXT((#3689,#3691,#3692))
REPRESENTATION_CONTEXT('','3D')
);
#3676=(
GEOMETRIC_REPRESENTATION_CONTEXT(3)
GLOBAL_UNCERTAINTY_ASSIGNED_CONTEXT((#3659))
GLOBAL_UNIT_ASSIGNED_CONTEXT((#3689,#3691,#3692))
REPRESENTATION_CONTEXT('','3D')
);
#3677=(
GEOMETRIC_REPRESENTATION_CONTEXT(3)
GLOBAL_UNCERTAINTY_ASSIGNED_CONTEXT((#3660))
GLOBAL_UNIT_ASSIGNED_CONTEXT((#3689,#3691,#3692))
REPRESENTATION_CONTEXT('','3D')
);
#3678=(
GEOMETRIC_REPRESENTATION_CONTEXT(3)
GLOBAL_UNCERTAINTY_ASSIGNED_CONTEXT((#3661))
GLOBAL_UNIT_ASSIGNED_CONTEXT((#3689,#3691,#3692))
REPRESENTATION_CONTEXT('','3D')
);
#3679=(
GEOMETRIC_REPRESENTATION_CONTEXT(3)
GLOBAL_UNCERTAINTY_ASSIGNED_CONTEXT((#3662))
GLOBAL_UNIT_ASSIGNED_CONTEXT((#3689,#3691,#3692))
REPRESENTATION_CONTEXT('','3D')
);
#3680=(
GEOMETRIC_REPRESENTATION_CONTEXT(3)
GLOBAL_UNCERTAINTY_ASSIGNED_CONTEXT((#3663))
GLOBAL_UNIT_ASSIGNED_CONTEXT((#3689,#3691,#3692))
REPRESENTATION_CONTEXT('','3D')
);
#3681=(
GEOMETRIC_REPRESENTATION_CONTEXT(3)
GLOBAL_UNCERTAINTY_ASSIGNED_CONTEXT((#3664))
GLOBAL_UNIT_ASSIGNED_CONTEXT((#3689,#3691,#3692))
REPRESENTATION_CONTEXT('','3D')
);
#3682=(
GEOMETRIC_REPRESENTATION_CONTEXT(3)
GLOBAL_UNCERTAINTY_ASSIGNED_CONTEXT((#3665))
GLOBAL_UNIT_ASSIGNED_CONTEXT((#3689,#3691,#3692))
REPRESENTATION_CONTEXT('','3D')
);
#3683=(
GEOMETRIC_REPRESENTATION_CONTEXT(3)
GLOBAL_UNCERTAINTY_ASSIGNED_CONTEXT((#3666))
GLOBAL_UNIT_ASSIGNED_CONTEXT((#3689,#3691,#3692))
REPRESENTATION_CONTEXT('','3D')
);
#3684=(
GEOMETRIC_REPRESENTATION_CONTEXT(3)
GLOBAL_UNCERTAINTY_ASSIGNED_CONTEXT((#3667))
GLOBAL_UNIT_ASSIGNED_CONTEXT((#3689,#3691,#3692))
REPRESENTATION_CONTEXT('','3D')
);
#3685=(
GEOMETRIC_REPRESENTATION_CONTEXT(3)
GLOBAL_UNCERTAINTY_ASSIGNED_CONTEXT((#3668))
GLOBAL_UNIT_ASSIGNED_CONTEXT((#3689,#3691,#3692))
REPRESENTATION_CONTEXT('','3D')
);
#3686=(
GEOMETRIC_REPRESENTATION_CONTEXT(3)
GLOBAL_UNCERTAINTY_ASSIGNED_CONTEXT((#3669))
GLOBAL_UNIT_ASSIGNED_CONTEXT((#3689,#3691,#3692))
REPRESENTATION_CONTEXT('','3D')
);
#3687=(
GEOMETRIC_REPRESENTATION_CONTEXT(3)
GLOBAL_UNCERTAINTY_ASSIGNED_CONTEXT((#3670))
GLOBAL_UNIT_ASSIGNED_CONTEXT((#3689,#3691,#3692))
REPRESENTATION_CONTEXT('','3D')
);
#3688=(
GEOMETRIC_REPRESENTATION_CONTEXT(3)
GLOBAL_UNCERTAINTY_ASSIGNED_CONTEXT((#3671))
GLOBAL_UNIT_ASSIGNED_CONTEXT((#3689,#3691,#3692))
REPRESENTATION_CONTEXT('','3D')
);
#3689=(
LENGTH_UNIT()
NAMED_UNIT(*)
SI_UNIT(.CENTI.,.METRE.)
);
#3690=(
LENGTH_UNIT()
NAMED_UNIT(*)
SI_UNIT($,.METRE.)
);
#3691=(
NAMED_UNIT(*)
PLANE_ANGLE_UNIT()
SI_UNIT($,.RADIAN.)
);
#3692=(
NAMED_UNIT(*)
SI_UNIT($,.STERADIAN.)
SOLID_ANGLE_UNIT()
);
#3693=SHAPE_DEFINITION_REPRESENTATION(#3709,#3743);
#3694=SHAPE_DEFINITION_REPRESENTATION(#3710,#3744);
#3695=SHAPE_DEFINITION_REPRESENTATION(#3711,#3745);
#3696=SHAPE_DEFINITION_REPRESENTATION(#3712,#3746);
#3697=SHAPE_DEFINITION_REPRESENTATION(#3713,#3747);
#3698=SHAPE_DEFINITION_REPRESENTATION(#3714,#3748);
#3699=SHAPE_DEFINITION_REPRESENTATION(#3715,#3749);
#3700=SHAPE_DEFINITION_REPRESENTATION(#3722,#3750);
#3701=SHAPE_DEFINITION_REPRESENTATION(#3723,#3751);
#3702=SHAPE_DEFINITION_REPRESENTATION(#3724,#3752);
#3703=SHAPE_DEFINITION_REPRESENTATION(#3725,#3753);
#3704=SHAPE_DEFINITION_REPRESENTATION(#3726,#3754);
#3705=SHAPE_DEFINITION_REPRESENTATION(#3727,#3755);
#3706=SHAPE_DEFINITION_REPRESENTATION(#3728,#3756);
#3707=SHAPE_DEFINITION_REPRESENTATION(#3729,#3757);
#3708=SHAPE_DEFINITION_REPRESENTATION(#3735,#3758);
#3709=PRODUCT_DEFINITION_SHAPE('',$,#3760);
#3710=PRODUCT_DEFINITION_SHAPE('',$,#3761);
#3711=PRODUCT_DEFINITION_SHAPE('',$,#3762);
#3712=PRODUCT_DEFINITION_SHAPE('',$,#3763);
#3713=PRODUCT_DEFINITION_SHAPE('',$,#3764);
#3714=PRODUCT_DEFINITION_SHAPE('',$,#3765);
#3715=PRODUCT_DEFINITION_SHAPE('',$,#3766);
#3716=PRODUCT_DEFINITION_SHAPE($,$,#95);
#3717=PRODUCT_DEFINITION_SHAPE($,$,#96);
#3718=PRODUCT_DEFINITION_SHAPE($,$,#97);
#3719=PRODUCT_DEFINITION_SHAPE($,$,#98);
#3720=PRODUCT_DEFINITION_SHAPE($,$,#99);
#3721=PRODUCT_DEFINITION_SHAPE($,$,#100);
#3722=PRODUCT_DEFINITION_SHAPE('',$,#3767);
#3723=PRODUCT_DEFINITION_SHAPE('',$,#3768);
#3724=PRODUCT_DEFINITION_SHAPE('',$,#3769);
#3725=PRODUCT_DEFINITION_SHAPE('',$,#3770);
#3726=PRODUCT_DEFINITION_SHAPE('',$,#3771);
#3727=PRODUCT_DEFINITION_SHAPE('',$,#3772);
#3728=PRODUCT_DEFINITION_SHAPE('',$,#3773);
#3729=PRODUCT_DEFINITION_SHAPE('',$,#3774);
#3730=PRODUCT_DEFINITION_SHAPE($,$,#101);
#3731=PRODUCT_DEFINITION_SHAPE($,$,#102);
#3732=PRODUCT_DEFINITION_SHAPE($,$,#103);
#3733=PRODUCT_DEFINITION_SHAPE($,$,#104);
#3734=PRODUCT_DEFINITION_SHAPE($,$,#105);
#3735=PRODUCT_DEFINITION_SHAPE('',$,#3775);
#3736=PRODUCT_DEFINITION_SHAPE($,$,#106);
#3737=PRODUCT_DEFINITION_SHAPE($,$,#107);
#3738=PRODUCT_DEFINITION_SHAPE($,$,#108);
#3739=PRODUCT_DEFINITION_SHAPE($,$,#109);
#3740=PRODUCT_DEFINITION_SHAPE($,$,#110);
#3741=PRODUCT_DEFINITION_SHAPE($,$,#111);
#3742=PRODUCT_DEFINITION_SHAPE($,$,#112);
#3743=SHAPE_REPRESENTATION('',(#1960,#2219,#2220),#3672);
#3744=SHAPE_REPRESENTATION('',(#1961,#2053,#2054,#2055,#2056,#2057,#2058),
#3673);
#3745=SHAPE_REPRESENTATION('',(#1962),#3674);
#3746=SHAPE_REPRESENTATION('',(#1997),#3675);
#3747=SHAPE_REPRESENTATION('',(#2011),#3676);
#3748=SHAPE_REPRESENTATION('',(#2020),#3677);
#3749=SHAPE_REPRESENTATION('',(#2029),#3678);
#3750=SHAPE_REPRESENTATION('',(#2059,#2214,#2215,#2216,#2217,#2218),#3679);
#3751=SHAPE_REPRESENTATION('',(#2060),#3680);
#3752=SHAPE_REPRESENTATION('',(#2077,#2200,#2201,#2202,#2203,#2204),#3681);
#3753=SHAPE_REPRESENTATION('',(#2078),#3682);
#3754=SHAPE_REPRESENTATION('',(#2098),#3683);
#3755=SHAPE_REPRESENTATION('',(#2118),#3684);
#3756=SHAPE_REPRESENTATION('',(#2133),#3685);
#3757=SHAPE_REPRESENTATION('',(#2183),#3686);
#3758=SHAPE_REPRESENTATION('',(#2205),#3687);
#3759=PRODUCT_DEFINITION_CONTEXT('part definition',#3809,'design');
#3760=PRODUCT_DEFINITION('PAT-038',
'PAT-038',#3776,#3759);
#3761=PRODUCT_DEFINITION('Fork and fixed twelve millimetre axle',
'Fork and fixed twelve millimetre axle',#3777,#3759);
#3762=PRODUCT_DEFINITION('Mounting fork','Mounting fork',#3778,#3759);
#3763=PRODUCT_DEFINITION('Twelve millimetre dead axle',
'Twelve millimetre dead axle',#3779,#3759);
#3764=PRODUCT_DEFINITION('Inner race spacer','Inner race spacer',#3780,
#3759);
#3765=PRODUCT_DEFINITION('Axle keeper','Axle keeper',#3781,#3759);
#3766=PRODUCT_DEFINITION('M4x10 Cap Screw','M4x10 Cap Screw',#3782,#3759);
#3767=PRODUCT_DEFINITION('Fifty millimetre roller',
'Fifty millimetre roller',#3783,#3759);
#3768=PRODUCT_DEFINITION('Fifty millimetre wheel',
'Fifty millimetre wheel',#3784,#3759);
#3769=PRODUCT_DEFINITION('Sealed Ball Bearing - 12 x 32 x 10 mm',
'Sealed Ball Bearing - 12 x 32 x 10 mm',#3785,#3759);
#3770=PRODUCT_DEFINITION('Inner ring','Inner ring',#3786,#3759);
#3771=PRODUCT_DEFINITION('Outer ring','Outer ring',#3787,#3759);
#3772=PRODUCT_DEFINITION('Balls','Balls',#3788,#3759);
#3773=PRODUCT_DEFINITION('Cage','Cage',#3789,#3759);
#3774=PRODUCT_DEFINITION('Seals 2RS','Seals 2RS',#3790,#3759);
#3775=PRODUCT_DEFINITION('Bearing end retainer','Bearing end retainer',
#3791,#3759);
#3776=PRODUCT_DEFINITION_FORMATION('',$,#3811);
#3777=PRODUCT_DEFINITION_FORMATION('',$,#3812);
#3778=PRODUCT_DEFINITION_FORMATION('',$,#3813);
#3779=PRODUCT_DEFINITION_FORMATION('',$,#3814);
#3780=PRODUCT_DEFINITION_FORMATION('',$,#3815);
#3781=PRODUCT_DEFINITION_FORMATION('',$,#3816);
#3782=PRODUCT_DEFINITION_FORMATION('',$,#3817);
#3783=PRODUCT_DEFINITION_FORMATION('',$,#3818);
#3784=PRODUCT_DEFINITION_FORMATION('',$,#3819);
#3785=PRODUCT_DEFINITION_FORMATION('',$,#3820);
#3786=PRODUCT_DEFINITION_FORMATION('',$,#3821);
#3787=PRODUCT_DEFINITION_FORMATION('',$,#3822);
#3788=PRODUCT_DEFINITION_FORMATION('',$,#3823);
#3789=PRODUCT_DEFINITION_FORMATION('',$,#3824);
#3790=PRODUCT_DEFINITION_FORMATION('',$,#3825);
#3791=PRODUCT_DEFINITION_FORMATION('',$,#3826);
#3792=PRODUCT_RELATED_PRODUCT_CATEGORY('PAT-038',
'PAT-038',(#3811));
#3793=PRODUCT_RELATED_PRODUCT_CATEGORY(
'Fork and fixed twelve millimetre axle',
'Fork and fixed twelve millimetre axle',(#3812));
#3794=PRODUCT_RELATED_PRODUCT_CATEGORY('Mounting fork','Mounting fork',
(#3813));
#3795=PRODUCT_RELATED_PRODUCT_CATEGORY('Twelve millimetre dead axle',
'Twelve millimetre dead axle',(#3814));
#3796=PRODUCT_RELATED_PRODUCT_CATEGORY('Inner race spacer',
'Inner race spacer',(#3815));
#3797=PRODUCT_RELATED_PRODUCT_CATEGORY('Axle keeper','Axle keeper',(#3816));
#3798=PRODUCT_RELATED_PRODUCT_CATEGORY('M4x10 Cap Screw',
'M4x10 Cap Screw',(#3817));
#3799=PRODUCT_RELATED_PRODUCT_CATEGORY('Fifty millimetre roller',
'Fifty millimetre roller',(#3818));
#3800=PRODUCT_RELATED_PRODUCT_CATEGORY('Fifty millimetre wheel',
'Fifty millimetre wheel',(#3819));
#3801=PRODUCT_RELATED_PRODUCT_CATEGORY(
'Sealed Ball Bearing - 12 x 32 x 10 mm',
'Sealed Ball Bearing - 12 x 32 x 10 mm',(#3820));
#3802=PRODUCT_RELATED_PRODUCT_CATEGORY('Inner ring','Inner ring',(#3821));
#3803=PRODUCT_RELATED_PRODUCT_CATEGORY('Outer ring','Outer ring',(#3822));
#3804=PRODUCT_RELATED_PRODUCT_CATEGORY('Balls','Balls',(#3823));
#3805=PRODUCT_RELATED_PRODUCT_CATEGORY('Cage','Cage',(#3824));
#3806=PRODUCT_RELATED_PRODUCT_CATEGORY('Seals 2RS','Seals 2RS',(#3825));
#3807=PRODUCT_RELATED_PRODUCT_CATEGORY('Bearing end retainer',
'Bearing end retainer',(#3826));
#3808=APPLICATION_PROTOCOL_DEFINITION('international standard',
'automotive_design',2009,#3809);
#3809=APPLICATION_CONTEXT(
'Core Data for Automotive Mechanical Design Process');
#3810=PRODUCT_CONTEXT('part definition',#3809,'mechanical');
#3811=PRODUCT('PAT-038','PAT-038',
'PAT-038',(#3810));
#3812=PRODUCT('Fork and fixed twelve millimetre axle',
'Fork and fixed twelve millimetre axle',
'Fork and fixed twelve millimetre axle',(#3810));
#3813=PRODUCT('Mounting fork','Mounting fork','Mounting fork',(#3810));
#3814=PRODUCT('Twelve millimetre dead axle',
'Twelve millimetre dead axle','Twelve millimetre dead axle',(#3810));
#3815=PRODUCT('Inner race spacer','Inner race spacer',
'Inner race spacer',(#3810));
#3816=PRODUCT('Axle keeper','Axle keeper','Axle keeper',(#3810));
#3817=PRODUCT('M4x10 Cap Screw','M4x10 Cap Screw','M4x10 Cap Screw',(#3810));
#3818=PRODUCT('Fifty millimetre roller','Fifty millimetre roller',
'Fifty millimetre roller',(#3810));
#3819=PRODUCT('Fifty millimetre wheel','Fifty millimetre wheel',
'Fifty millimetre wheel',(#3810));
#3820=PRODUCT('Sealed Ball Bearing - 12 x 32 x 10 mm',
'Sealed Ball Bearing - 12 x 32 x 10 mm',
'Sealed Ball Bearing - 12 x 32 x 10 mm',(#3810));
#3821=PRODUCT('Inner ring','Inner ring','Inner ring',(#3810));
#3822=PRODUCT('Outer ring','Outer ring','Outer ring',(#3810));
#3823=PRODUCT('Balls','Balls','Balls',(#3810));
#3824=PRODUCT('Cage','Cage','Cage',(#3810));
#3825=PRODUCT('Seals 2RS','Seals 2RS','Seals 2RS',(#3810));
#3826=PRODUCT('Bearing end retainer','Bearing end retainer',
'Bearing end retainer',(#3810));
#3827=PRESENTATION_STYLE_ASSIGNMENT((#3833));
#3828=PRESENTATION_STYLE_ASSIGNMENT((#3834));
#3829=PRESENTATION_STYLE_ASSIGNMENT((#3835));
#3830=PRESENTATION_STYLE_ASSIGNMENT((#3836));
#3831=PRESENTATION_STYLE_ASSIGNMENT((#3837));
#3832=PRESENTATION_STYLE_ASSIGNMENT((#3838));
#3833=SURFACE_STYLE_USAGE(.BOTH.,#3839);
#3834=SURFACE_STYLE_USAGE(.BOTH.,#3840);
#3835=SURFACE_STYLE_USAGE(.BOTH.,#3841);
#3836=SURFACE_STYLE_USAGE(.BOTH.,#3842);
#3837=SURFACE_STYLE_USAGE(.BOTH.,#3843);
#3838=SURFACE_STYLE_USAGE(.BOTH.,#3844);
#3839=SURFACE_SIDE_STYLE('',(#3845));
#3840=SURFACE_SIDE_STYLE('',(#3846));
#3841=SURFACE_SIDE_STYLE('',(#3847));
#3842=SURFACE_SIDE_STYLE('',(#3848));
#3843=SURFACE_SIDE_STYLE('',(#3849));
#3844=SURFACE_SIDE_STYLE('',(#3850));
#3845=SURFACE_STYLE_FILL_AREA(#3851);
#3846=SURFACE_STYLE_FILL_AREA(#3852);
#3847=SURFACE_STYLE_FILL_AREA(#3853);
#3848=SURFACE_STYLE_FILL_AREA(#3854);
#3849=SURFACE_STYLE_FILL_AREA(#3855);
#3850=SURFACE_STYLE_FILL_AREA(#3856);
#3851=FILL_AREA_STYLE('Steel - Satin',(#3857));
#3852=FILL_AREA_STYLE('CAD Library Painted - Engineering blue',(#3858));
#3853=FILL_AREA_STYLE('CAD Library Painted - Steel gray',(#3859));
#3854=FILL_AREA_STYLE('CAD Library Painted - Graphite',(#3860));
#3855=FILL_AREA_STYLE('CAD Library Painted - Light blue',(#3861));
#3856=FILL_AREA_STYLE('CAD Library Painted - Off white',(#3862));
#3857=FILL_AREA_STYLE_COLOUR('Steel - Satin',#3863);
#3858=FILL_AREA_STYLE_COLOUR('CAD Library Painted - Engineering blue',#3864);
#3859=FILL_AREA_STYLE_COLOUR('CAD Library Painted - Steel gray',#3865);
#3860=FILL_AREA_STYLE_COLOUR('CAD Library Painted - Graphite',#3866);
#3861=FILL_AREA_STYLE_COLOUR('CAD Library Painted - Light blue',#3867);
#3862=FILL_AREA_STYLE_COLOUR('CAD Library Painted - Off white',#3868);
#3863=COLOUR_RGB('Steel - Satin',0.627450980392157,0.627450980392157,0.627450980392157);
#3864=COLOUR_RGB('CAD Library Painted - Engineering blue',0.12156862745098,
0.356862745098039,0.6);
#3865=COLOUR_RGB('CAD Library Painted - Steel gray',0.592156862745098,0.631372549019608,
0.67843137254902);
#3866=COLOUR_RGB('CAD Library Painted - Graphite',0.0980392156862745,0.109803921568627,
0.125490196078431);
#3867=COLOUR_RGB('CAD Library Painted - Light blue',0.286274509803922,0.552941176470588,
0.780392156862745);
#3868=COLOUR_RGB('CAD Library Painted - Off white',0.909803921568627,0.901960784313726,
0.858823529411765);
#3869=COLOUR_RGB('Dark Blue',0.08,0.2,0.34);
#3870=FILL_AREA_STYLE_COLOUR('',#3869);
#3871=FILL_AREA_STYLE('',(#3870));
#3872=SURFACE_STYLE_FILL_AREA(#3871);
#3873=SURFACE_SIDE_STYLE('',(#3872));
#3874=SURFACE_STYLE_USAGE(.BOTH.,#3873);
#3875=PRESENTATION_STYLE_ASSIGNMENT((#3874));
#3876=COLOUR_RGB('Light Blue',0.38,0.62,0.78);
#3877=FILL_AREA_STYLE_COLOUR('',#3876);
#3878=FILL_AREA_STYLE('',(#3877));
#3879=SURFACE_STYLE_FILL_AREA(#3878);
#3880=SURFACE_SIDE_STYLE('',(#3879));
#3881=SURFACE_STYLE_USAGE(.BOTH.,#3880);
#3882=PRESENTATION_STYLE_ASSIGNMENT((#3881));
#3883=COLOUR_RGB('Sky Blue',0.24,0.69,0.87);
#3884=FILL_AREA_STYLE_COLOUR('',#3883);
#3885=FILL_AREA_STYLE('',(#3884));
#3886=SURFACE_STYLE_FILL_AREA(#3885);
#3887=SURFACE_SIDE_STYLE('',(#3886));
#3888=SURFACE_STYLE_USAGE(.BOTH.,#3887);
#3889=PRESENTATION_STYLE_ASSIGNMENT((#3888));
#3890=COLOUR_RGB('Grey',0.48,0.52,0.57);
#3891=FILL_AREA_STYLE_COLOUR('',#3890);
#3892=FILL_AREA_STYLE('',(#3891));
#3893=SURFACE_STYLE_FILL_AREA(#3892);
#3894=SURFACE_SIDE_STYLE('',(#3893));
#3895=SURFACE_STYLE_USAGE(.BOTH.,#3894);
#3896=PRESENTATION_STYLE_ASSIGNMENT((#3895));
#3897=COLOUR_RGB('Black',0.12,0.14,0.17);
#3898=FILL_AREA_STYLE_COLOUR('',#3897);
#3899=FILL_AREA_STYLE('',(#3898));
#3900=SURFACE_STYLE_FILL_AREA(#3899);
#3901=SURFACE_SIDE_STYLE('',(#3900));
#3902=SURFACE_STYLE_USAGE(.BOTH.,#3901);
#3903=PRESENTATION_STYLE_ASSIGNMENT((#3902));
#3904=COLOUR_RGB('Off White',0.89,0.88,0.83);
#3905=FILL_AREA_STYLE_COLOUR('',#3904);
#3906=FILL_AREA_STYLE('',(#3905));
#3907=SURFACE_STYLE_FILL_AREA(#3906);
#3908=SURFACE_SIDE_STYLE('',(#3907));
#3909=SURFACE_STYLE_USAGE(.BOTH.,#3908);
#3910=PRESENTATION_STYLE_ASSIGNMENT((#3909));
ENDSEC;
END-ISO-10303-21;
